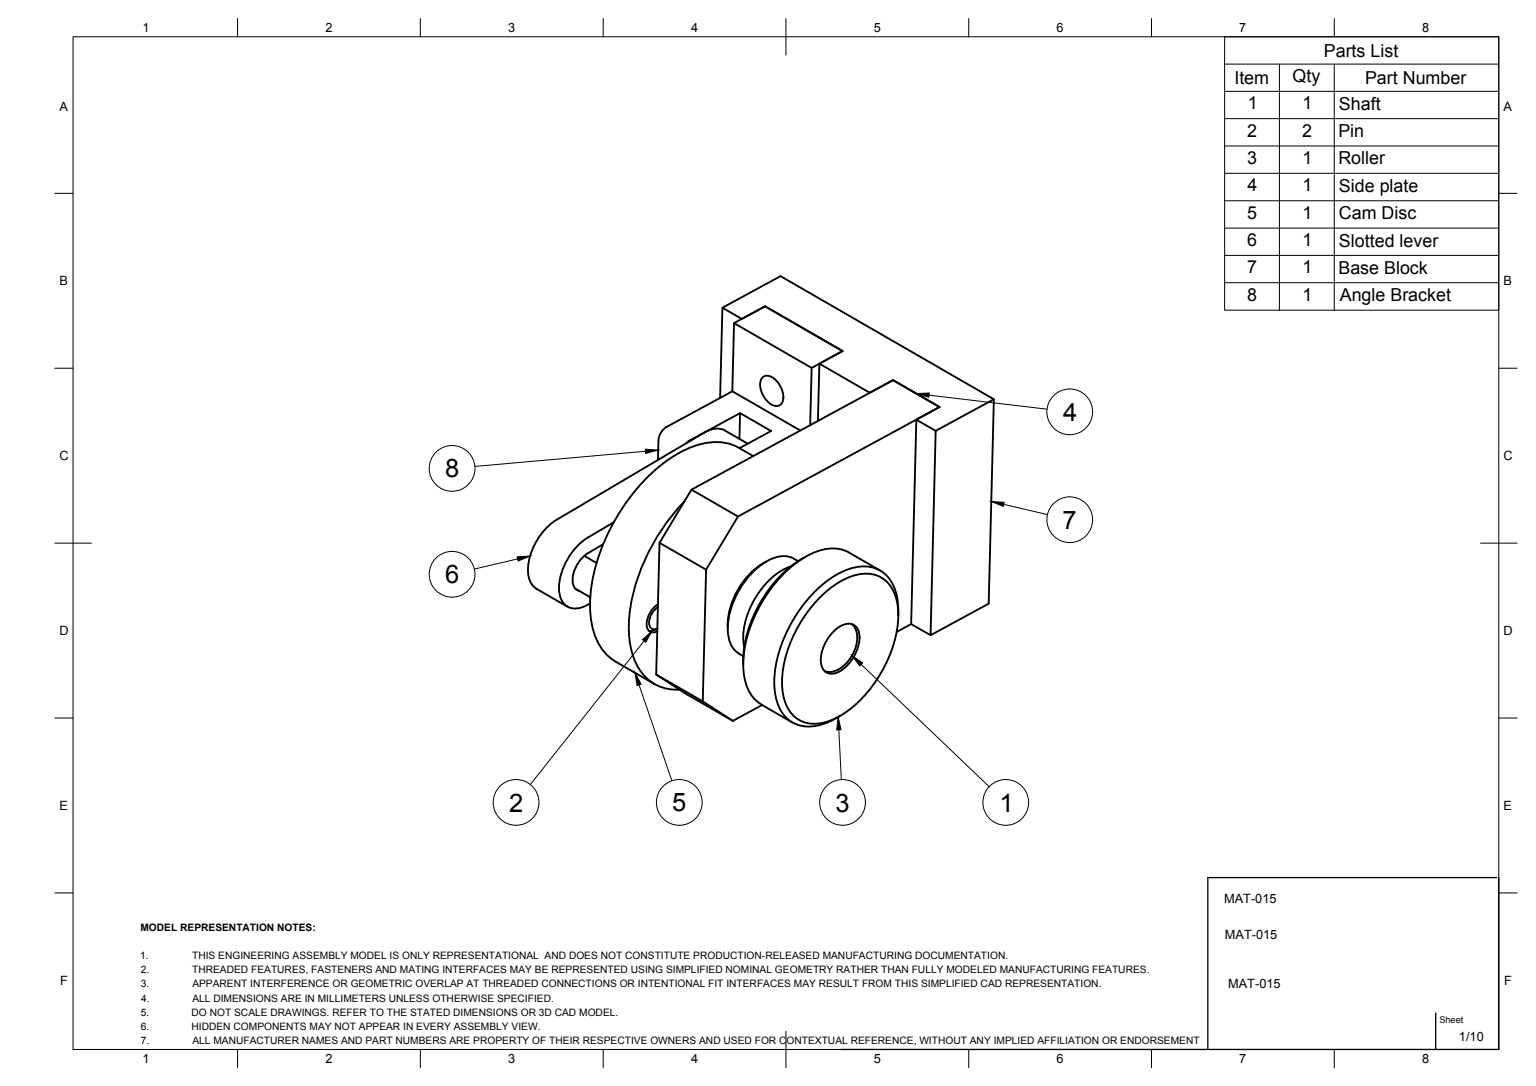
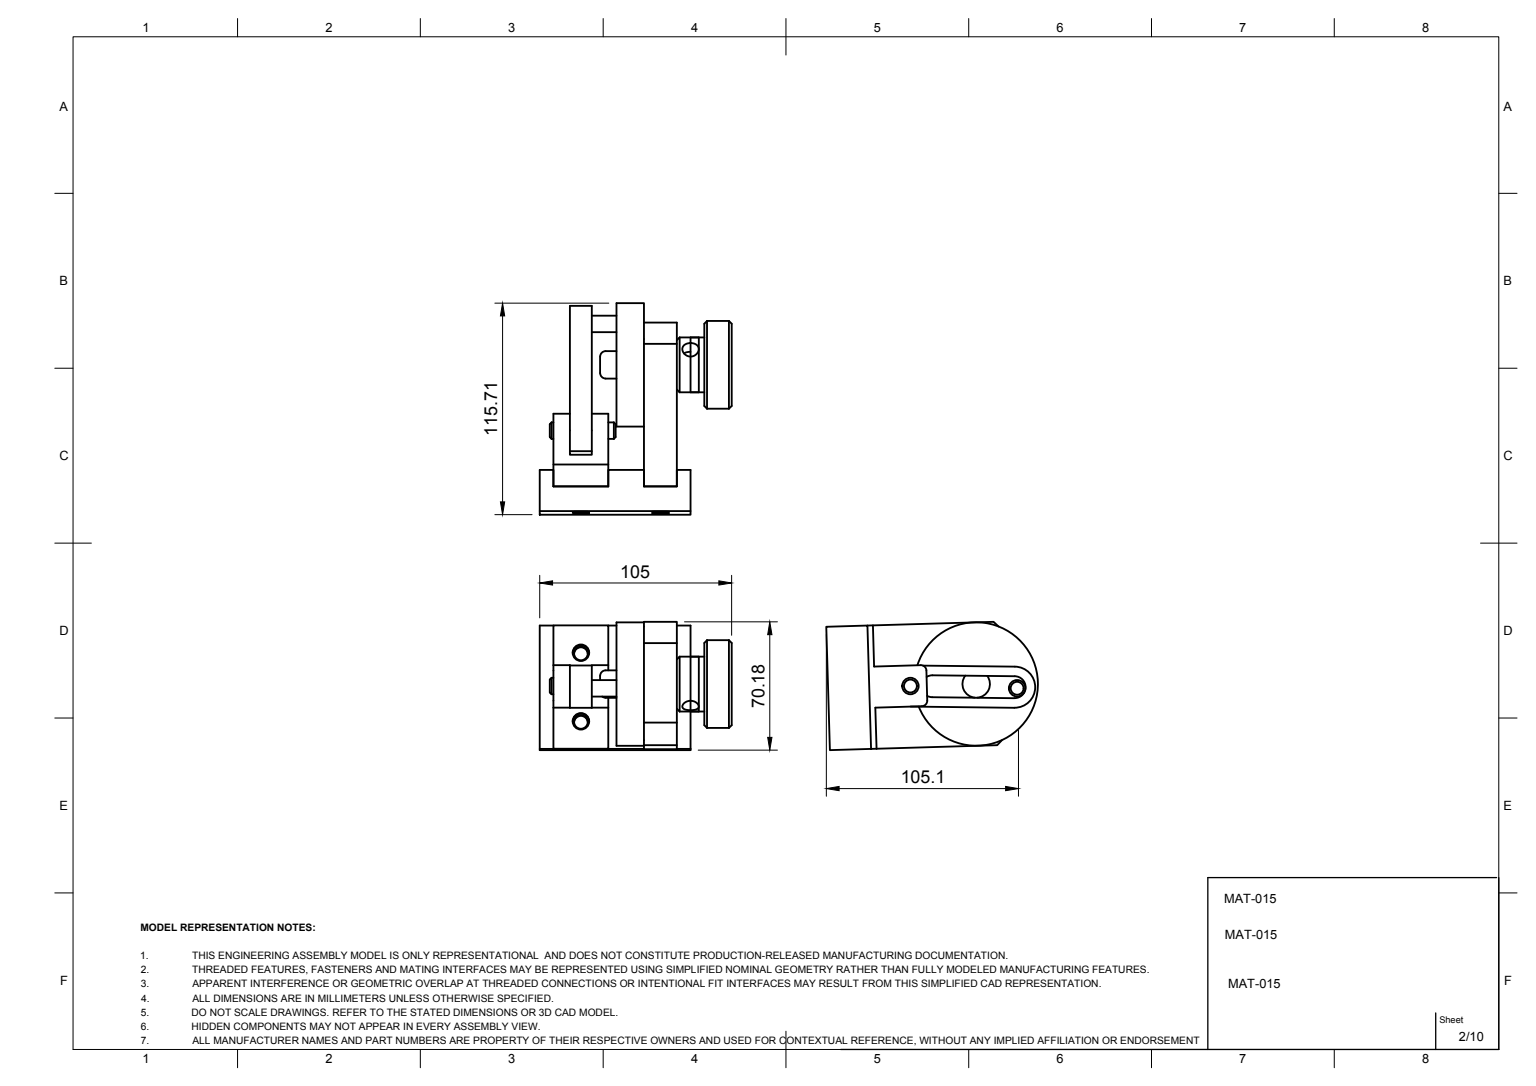
ISO-10303-21;
HEADER;
/* Generated by software containing ST-Developer
 * from STEP Tools, Inc. (www.steptools.com) 
 */

FILE_DESCRIPTION(
/* description */ ('STEP AP214'),
/* implementation_level */ '2;1');

FILE_NAME(
/* name */ 'MAT-015.step',
/* time_stamp */ '2026-11-14T06:03:18-08:00',
/* author */ (''),
/* organization */ (''),
/* preprocessor_version */ 'ST-DEVELOPER v20.2',
/* originating_system */ 'Autodesk Translation Framework v15.17.0.0',
/* authorisation */ '');

FILE_SCHEMA (('AUTOMOTIVE_DESIGN { 1 0 10303 214 3 1 1 }'));
ENDSEC;

DATA;
#10=MECHANICAL_DESIGN_GEOMETRIC_PRESENTATION_REPRESENTATION('',(#72,#73,
#74,#75,#76,#77,#78,#79),#3206);
#11=ITEM_DEFINED_TRANSFORMATION($,$,#1877,#2066);
#12=ITEM_DEFINED_TRANSFORMATION($,$,#2055,#2067);
#13=ITEM_DEFINED_TRANSFORMATION($,$,#1903,#2068);
#14=ITEM_DEFINED_TRANSFORMATION($,$,#1925,#2069);
#15=ITEM_DEFINED_TRANSFORMATION($,$,#1949,#2070);
#16=ITEM_DEFINED_TRANSFORMATION($,$,#1961,#2071);
#17=ITEM_DEFINED_TRANSFORMATION($,$,#1983,#2072);
#18=ITEM_DEFINED_TRANSFORMATION($,$,#2016,#2073);
#19=ITEM_DEFINED_TRANSFORMATION($,$,#2055,#2074);
#20=(
REPRESENTATION_RELATIONSHIP($,$,#3239,#3238)
REPRESENTATION_RELATIONSHIP_WITH_TRANSFORMATION(#11)
SHAPE_REPRESENTATION_RELATIONSHIP()
);
#21=(
REPRESENTATION_RELATIONSHIP($,$,#3246,#3238)
REPRESENTATION_RELATIONSHIP_WITH_TRANSFORMATION(#12)
SHAPE_REPRESENTATION_RELATIONSHIP()
);
#22=(
REPRESENTATION_RELATIONSHIP($,$,#3240,#3238)
REPRESENTATION_RELATIONSHIP_WITH_TRANSFORMATION(#13)
SHAPE_REPRESENTATION_RELATIONSHIP()
);
#23=(
REPRESENTATION_RELATIONSHIP($,$,#3241,#3238)
REPRESENTATION_RELATIONSHIP_WITH_TRANSFORMATION(#14)
SHAPE_REPRESENTATION_RELATIONSHIP()
);
#24=(
REPRESENTATION_RELATIONSHIP($,$,#3242,#3238)
REPRESENTATION_RELATIONSHIP_WITH_TRANSFORMATION(#15)
SHAPE_REPRESENTATION_RELATIONSHIP()
);
#25=(
REPRESENTATION_RELATIONSHIP($,$,#3243,#3238)
REPRESENTATION_RELATIONSHIP_WITH_TRANSFORMATION(#16)
SHAPE_REPRESENTATION_RELATIONSHIP()
);
#26=(
REPRESENTATION_RELATIONSHIP($,$,#3244,#3238)
REPRESENTATION_RELATIONSHIP_WITH_TRANSFORMATION(#17)
SHAPE_REPRESENTATION_RELATIONSHIP()
);
#27=(
REPRESENTATION_RELATIONSHIP($,$,#3245,#3238)
REPRESENTATION_RELATIONSHIP_WITH_TRANSFORMATION(#18)
SHAPE_REPRESENTATION_RELATIONSHIP()
);
#28=(
REPRESENTATION_RELATIONSHIP($,$,#3246,#3238)
REPRESENTATION_RELATIONSHIP_WITH_TRANSFORMATION(#19)
SHAPE_REPRESENTATION_RELATIONSHIP()
);
#29=CONTEXT_DEPENDENT_SHAPE_REPRESENTATION(#20,#3229);
#30=CONTEXT_DEPENDENT_SHAPE_REPRESENTATION(#21,#3230);
#31=CONTEXT_DEPENDENT_SHAPE_REPRESENTATION(#22,#3231);
#32=CONTEXT_DEPENDENT_SHAPE_REPRESENTATION(#23,#3232);
#33=CONTEXT_DEPENDENT_SHAPE_REPRESENTATION(#24,#3233);
#34=CONTEXT_DEPENDENT_SHAPE_REPRESENTATION(#25,#3234);
#35=CONTEXT_DEPENDENT_SHAPE_REPRESENTATION(#26,#3235);
#36=CONTEXT_DEPENDENT_SHAPE_REPRESENTATION(#27,#3236);
#37=CONTEXT_DEPENDENT_SHAPE_REPRESENTATION(#28,#3237);
#38=NEXT_ASSEMBLY_USAGE_OCCURRENCE('Shaft:1','Shaft:1','Shaft:1',#3248,
#3249,'Shaft:1');
#39=NEXT_ASSEMBLY_USAGE_OCCURRENCE('Pin:1','Pin:1','Pin:1',#3248,#3256,
'Pin:1');
#40=NEXT_ASSEMBLY_USAGE_OCCURRENCE('Roller:1','Roller:1','Roller:1',#3248,
#3250,'Roller:1');
#41=NEXT_ASSEMBLY_USAGE_OCCURRENCE('Side Plate:1','Side Plate:1',
'Side Plate:1',#3248,#3251,'Side Plate:1');
#42=NEXT_ASSEMBLY_USAGE_OCCURRENCE('Cam Disc:1','Cam Disc:1',
'Cam Disc:1',#3248,#3252,'Cam Disc:1');
#43=NEXT_ASSEMBLY_USAGE_OCCURRENCE('Slotted Lever:1','Slotted Lever:1',
'Slotted Lever:1',#3248,#3253,'Slotted Lever:1');
#44=NEXT_ASSEMBLY_USAGE_OCCURRENCE('Base Block:1','Base Block:1',
'Base Block:1',#3248,#3254,'Base Block:1');
#45=NEXT_ASSEMBLY_USAGE_OCCURRENCE('Angle Bracket:1','Angle Bracket:1',
'Angle Bracket:1',#3248,#3255,'Angle Bracket:1');
#46=NEXT_ASSEMBLY_USAGE_OCCURRENCE('Pin:2','Pin:2','Pin:2',#3248,#3256,
'Pin:2');
#47=B_SPLINE_CURVE_WITH_KNOTS('',3,(#2691,#2692,#2693,#2694,#2695,#2696,
#2697,#2698,#2699,#2700,#2701,#2702,#2703,#2704,#2705,#2706,#2707,#2708),
 .UNSPECIFIED.,.F.,.F.,(4,2,2,2,2,2,2,2,4),(-1.36519473470625,-1.19451997041109,
-1.02384520611593,-0.853221286734528,-0.682597367353127,-0.511973447971726,
-0.341349528590325,-0.170674764295162,0.),.UNSPECIFIED.);
#48=B_SPLINE_CURVE_WITH_KNOTS('',3,(#2712,#2713,#2714,#2715,#2716,#2717,
#2718,#2719,#2720,#2721,#2722,#2723,#2724,#2725,#2726,#2727,#2728,#2729),
 .UNSPECIFIED.,.F.,.F.,(4,2,2,2,2,2,2,2,4),(-1.39899108486948,-1.22355122072177,
-1.04811135657406,-0.873803449504402,-0.699495542434742,-0.525187635365083,
-0.350879728295424,-0.175439864147712,0.),.UNSPECIFIED.);
#49=B_SPLINE_CURVE_WITH_KNOTS('',3,(#2730,#2731,#2732,#2733,#2734,#2735,
#2736,#2737,#2738,#2739,#2740,#2741,#2742,#2743,#2744,#2745,#2746,#2747),
 .UNSPECIFIED.,.F.,.F.,(4,2,2,2,2,2,2,2,4),(-2.79798216973897,-2.62254230559126,
-2.44710244144355,-2.27279453437389,-2.09848662730423,-1.92417872023457,
-1.74987081316491,-1.5744309490172,-1.39899108486948),.UNSPECIFIED.);
#50=B_SPLINE_CURVE_WITH_KNOTS('',3,(#2748,#2749,#2750,#2751,#2752,#2753,
#2754,#2755,#2756,#2757,#2758,#2759,#2760,#2761,#2762,#2763,#2764,#2765),
 .UNSPECIFIED.,.F.,.F.,(4,2,2,2,2,2,2,2,4),(0.,0.170674764295163,0.341349528590325,
0.511973447971726,0.682597367353127,0.853221286734528,1.02384520611593,
1.19451997041109,1.36519473470625),.UNSPECIFIED.);
#51=CONICAL_SURFACE('',#1904,13.5,0.785398163397445);
#52=CONICAL_SURFACE('',#1908,22.5,0.785398163397448);
#53=CONICAL_SURFACE('',#1912,24.,0.785398163397452);
#54=CONICAL_SURFACE('',#2056,4.50000000000002,0.785398163397454);
#55=CONICAL_SURFACE('',#2059,3.54000000000001,0.785398163397446);
#56=SHAPE_REPRESENTATION_RELATIONSHIP('SRR','None',#3239,#64);
#57=SHAPE_REPRESENTATION_RELATIONSHIP('SRR','None',#3240,#65);
#58=SHAPE_REPRESENTATION_RELATIONSHIP('SRR','None',#3241,#66);
#59=SHAPE_REPRESENTATION_RELATIONSHIP('SRR','None',#3242,#67);
#60=SHAPE_REPRESENTATION_RELATIONSHIP('SRR','None',#3243,#68);
#61=SHAPE_REPRESENTATION_RELATIONSHIP('SRR','None',#3244,#69);
#62=SHAPE_REPRESENTATION_RELATIONSHIP('SRR','None',#3245,#70);
#63=SHAPE_REPRESENTATION_RELATIONSHIP('SRR','None',#3246,#71);
#64=ADVANCED_BREP_SHAPE_REPRESENTATION('',(#80),#3198);
#65=ADVANCED_BREP_SHAPE_REPRESENTATION('',(#81),#3199);
#66=ADVANCED_BREP_SHAPE_REPRESENTATION('',(#82),#3200);
#67=ADVANCED_BREP_SHAPE_REPRESENTATION('',(#83),#3201);
#68=ADVANCED_BREP_SHAPE_REPRESENTATION('',(#84),#3202);
#69=ADVANCED_BREP_SHAPE_REPRESENTATION('',(#85),#3203);
#70=ADVANCED_BREP_SHAPE_REPRESENTATION('',(#86),#3204);
#71=ADVANCED_BREP_SHAPE_REPRESENTATION('',(#87),#3205);
#72=STYLED_ITEM('',(#3288),#80);
#73=STYLED_ITEM('',(#3288),#81);
#74=STYLED_ITEM('',(#3288),#82);
#75=STYLED_ITEM('',(#3289),#83);
#76=STYLED_ITEM('',(#3288),#84);
#77=STYLED_ITEM('',(#3289),#85);
#78=STYLED_ITEM('',(#3290),#86);
#79=STYLED_ITEM('',(#3290),#87);
#80=MANIFOLD_SOLID_BREP('Body1',#1779);
#81=MANIFOLD_SOLID_BREP('Body1',#1780);
#82=MANIFOLD_SOLID_BREP('Body1',#1781);
#83=MANIFOLD_SOLID_BREP('Body1',#1782);
#84=MANIFOLD_SOLID_BREP('Body1',#1783);
#85=MANIFOLD_SOLID_BREP('Body1',#1784);
#86=MANIFOLD_SOLID_BREP('Body1',#1785);
#87=MANIFOLD_SOLID_BREP('Body1',#1786);
#88=PLANE('',#1896);
#89=PLANE('',#1897);
#90=PLANE('',#1898);
#91=PLANE('',#1899);
#92=PLANE('',#1900);
#93=PLANE('',#1901);
#94=PLANE('',#1902);
#95=PLANE('',#1922);
#96=PLANE('',#1923);
#97=PLANE('',#1924);
#98=PLANE('',#1938);
#99=PLANE('',#1939);
#100=PLANE('',#1940);
#101=PLANE('',#1941);
#102=PLANE('',#1942);
#103=PLANE('',#1943);
#104=PLANE('',#1944);
#105=PLANE('',#1945);
#106=PLANE('',#1946);
#107=PLANE('',#1947);
#108=PLANE('',#1948);
#109=PLANE('',#1959);
#110=PLANE('',#1960);
#111=PLANE('',#1971);
#112=PLANE('',#1974);
#113=PLANE('',#1978);
#114=PLANE('',#1979);
#115=PLANE('',#1981);
#116=PLANE('',#1982);
#117=PLANE('',#2002);
#118=PLANE('',#2003);
#119=PLANE('',#2004);
#120=PLANE('',#2005);
#121=PLANE('',#2006);
#122=PLANE('',#2007);
#123=PLANE('',#2008);
#124=PLANE('',#2009);
#125=PLANE('',#2010);
#126=PLANE('',#2011);
#127=PLANE('',#2012);
#128=PLANE('',#2013);
#129=PLANE('',#2014);
#130=PLANE('',#2015);
#131=PLANE('',#2029);
#132=PLANE('',#2030);
#133=PLANE('',#2031);
#134=PLANE('',#2032);
#135=PLANE('',#2033);
#136=PLANE('',#2034);
#137=PLANE('',#2037);
#138=PLANE('',#2038);
#139=PLANE('',#2041);
#140=PLANE('',#2042);
#141=PLANE('',#2043);
#142=PLANE('',#2044);
#143=PLANE('',#2047);
#144=PLANE('',#2050);
#145=PLANE('',#2064);
#146=PLANE('',#2065);
#147=FACE_BOUND('',#617,.T.);
#148=FACE_BOUND('',#620,.T.);
#149=FACE_BOUND('',#622,.T.);
#150=FACE_BOUND('',#633,.T.);
#151=FACE_BOUND('',#635,.T.);
#152=FACE_BOUND('',#637,.T.);
#153=FACE_BOUND('',#639,.T.);
#154=FACE_BOUND('',#641,.T.);
#155=FACE_BOUND('',#647,.T.);
#156=FACE_BOUND('',#649,.T.);
#157=FACE_BOUND('',#652,.T.);
#158=FACE_BOUND('',#653,.T.);
#159=FACE_BOUND('',#654,.T.);
#160=FACE_BOUND('',#666,.T.);
#161=FACE_BOUND('',#667,.T.);
#162=FACE_BOUND('',#669,.T.);
#163=FACE_BOUND('',#670,.T.);
#164=FACE_BOUND('',#675,.T.);
#165=FACE_BOUND('',#676,.T.);
#166=FACE_BOUND('',#678,.T.);
#167=FACE_BOUND('',#679,.T.);
#168=FACE_BOUND('',#693,.T.);
#169=FACE_BOUND('',#694,.T.);
#170=FACE_BOUND('',#695,.T.);
#171=FACE_BOUND('',#697,.T.);
#172=FACE_BOUND('',#698,.T.);
#173=FACE_BOUND('',#699,.T.);
#174=FACE_BOUND('',#701,.T.);
#175=FACE_BOUND('',#702,.T.);
#176=FACE_BOUND('',#703,.T.);
#177=FACE_BOUND('',#704,.T.);
#178=FACE_BOUND('',#705,.T.);
#179=FACE_BOUND('',#706,.T.);
#180=FACE_BOUND('',#724,.T.);
#181=FACE_BOUND('',#726,.T.);
#182=FACE_BOUND('',#728,.T.);
#183=FACE_BOUND('',#729,.T.);
#184=FACE_BOUND('',#732,.T.);
#185=FACE_BOUND('',#735,.T.);
#186=FACE_BOUND('',#740,.T.);
#187=FACE_BOUND('',#742,.T.);
#188=LINE('',#2638,#333);
#189=LINE('',#2643,#334);
#190=LINE('',#2646,#335);
#191=LINE('',#2652,#336);
#192=LINE('',#2655,#337);
#193=LINE('',#2661,#338);
#194=LINE('',#2662,#339);
#195=LINE('',#2672,#340);
#196=LINE('',#2680,#341);
#197=LINE('',#2686,#342);
#198=LINE('',#2710,#343);
#199=LINE('',#2767,#344);
#200=LINE('',#2772,#345);
#201=LINE('',#2776,#346);
#202=LINE('',#2786,#347);
#203=LINE('',#2792,#348);
#204=LINE('',#2798,#349);
#205=LINE('',#2804,#350);
#206=LINE('',#2809,#351);
#207=LINE('',#2811,#352);
#208=LINE('',#2813,#353);
#209=LINE('',#2815,#354);
#210=LINE('',#2817,#355);
#211=LINE('',#2818,#356);
#212=LINE('',#2822,#357);
#213=LINE('',#2824,#358);
#214=LINE('',#2826,#359);
#215=LINE('',#2828,#360);
#216=LINE('',#2830,#361);
#217=LINE('',#2831,#362);
#218=LINE('',#2833,#363);
#219=LINE('',#2834,#364);
#220=LINE('',#2836,#365);
#221=LINE('',#2838,#366);
#222=LINE('',#2840,#367);
#223=LINE('',#2841,#368);
#224=LINE('',#2852,#369);
#225=LINE('',#2858,#370);
#226=LINE('',#2864,#371);
#227=LINE('',#2874,#372);
#228=LINE('',#2877,#373);
#229=LINE('',#2882,#374);
#230=LINE('',#2889,#375);
#231=LINE('',#2892,#376);
#232=LINE('',#2897,#377);
#233=LINE('',#2898,#378);
#234=LINE('',#2902,#379);
#235=LINE('',#2903,#380);
#236=LINE('',#2908,#381);
#237=LINE('',#2909,#382);
#238=LINE('',#2911,#383);
#239=LINE('',#2914,#384);
#240=LINE('',#2916,#385);
#241=LINE('',#2917,#386);
#242=LINE('',#2921,#387);
#243=LINE('',#2922,#388);
#244=LINE('',#2930,#389);
#245=LINE('',#2936,#390);
#246=LINE('',#2942,#391);
#247=LINE('',#2948,#392);
#248=LINE('',#2954,#393);
#249=LINE('',#2960,#394);
#250=LINE('',#2965,#395);
#251=LINE('',#2967,#396);
#252=LINE('',#2969,#397);
#253=LINE('',#2970,#398);
#254=LINE('',#2974,#399);
#255=LINE('',#2976,#400);
#256=LINE('',#2978,#401);
#257=LINE('',#2979,#402);
#258=LINE('',#2983,#403);
#259=LINE('',#2985,#404);
#260=LINE('',#2987,#405);
#261=LINE('',#2988,#406);
#262=LINE('',#2991,#407);
#263=LINE('',#2993,#408);
#264=LINE('',#2994,#409);
#265=LINE('',#2997,#410);
#266=LINE('',#2999,#411);
#267=LINE('',#3000,#412);
#268=LINE('',#3002,#413);
#269=LINE('',#3004,#414);
#270=LINE('',#3005,#415);
#271=LINE('',#3007,#416);
#272=LINE('',#3008,#417);
#273=LINE('',#3011,#418);
#274=LINE('',#3012,#419);
#275=LINE('',#3015,#420);
#276=LINE('',#3016,#421);
#277=LINE('',#3018,#422);
#278=LINE('',#3020,#423);
#279=LINE('',#3021,#424);
#280=LINE('',#3023,#425);
#281=LINE('',#3024,#426);
#282=LINE('',#3026,#427);
#283=LINE('',#3028,#428);
#284=LINE('',#3031,#429);
#285=LINE('',#3034,#430);
#286=LINE('',#3041,#431);
#287=LINE('',#3047,#432);
#288=LINE('',#3053,#433);
#289=LINE('',#3059,#434);
#290=LINE('',#3064,#435);
#291=LINE('',#3066,#436);
#292=LINE('',#3068,#437);
#293=LINE('',#3069,#438);
#294=LINE('',#3073,#439);
#295=LINE('',#3075,#440);
#296=LINE('',#3077,#441);
#297=LINE('',#3078,#442);
#298=LINE('',#3082,#443);
#299=LINE('',#3084,#444);
#300=LINE('',#3086,#445);
#301=LINE('',#3087,#446);
#302=LINE('',#3091,#447);
#303=LINE('',#3093,#448);
#304=LINE('',#3095,#449);
#305=LINE('',#3096,#450);
#306=LINE('',#3098,#451);
#307=LINE('',#3099,#452);
#308=LINE('',#3102,#453);
#309=LINE('',#3106,#454);
#310=LINE('',#3107,#455);
#311=LINE('',#3109,#456);
#312=LINE('',#3113,#457);
#313=LINE('',#3116,#458);
#314=LINE('',#3118,#459);
#315=LINE('',#3123,#460);
#316=LINE('',#3124,#461);
#317=LINE('',#3126,#462);
#318=LINE('',#3128,#463);
#319=LINE('',#3129,#464);
#320=LINE('',#3132,#465);
#321=LINE('',#3134,#466);
#322=LINE('',#3136,#467);
#323=LINE('',#3138,#468);
#324=LINE('',#3139,#469);
#325=LINE('',#3143,#470);
#326=LINE('',#3144,#471);
#327=LINE('',#3145,#472);
#328=LINE('',#3148,#473);
#329=LINE('',#3153,#474);
#330=LINE('',#3164,#475);
#331=LINE('',#3172,#476);
#332=LINE('',#3175,#477);
#333=VECTOR('',#2101,15.);
#334=VECTOR('',#2108,7.5);
#335=VECTOR('',#2111,7.49999999999999);
#336=VECTOR('',#2116,1000.);
#337=VECTOR('',#2119,1000.);
#338=VECTOR('',#2130,1000.);
#339=VECTOR('',#2131,1000.);
#340=VECTOR('',#2144,13.5);
#341=VECTOR('',#2153,22.5);
#342=VECTOR('',#2160,24.);
#343=VECTOR('',#2165,4.5);
#344=VECTOR('',#2168,24.);
#345=VECTOR('',#2173,7.5);
#346=VECTOR('',#2178,15.);
#347=VECTOR('',#2193,4.5);
#348=VECTOR('',#2200,3.75);
#349=VECTOR('',#2207,3.75);
#350=VECTOR('',#2214,7.50000000000001);
#351=VECTOR('',#2219,1000.);
#352=VECTOR('',#2220,1000.);
#353=VECTOR('',#2221,1000.);
#354=VECTOR('',#2222,1000.);
#355=VECTOR('',#2223,1000.);
#356=VECTOR('',#2224,1000.);
#357=VECTOR('',#2227,1000.);
#358=VECTOR('',#2228,1000.);
#359=VECTOR('',#2229,1000.);
#360=VECTOR('',#2230,1000.);
#361=VECTOR('',#2231,1000.);
#362=VECTOR('',#2232,1000.);
#363=VECTOR('',#2235,1000.);
#364=VECTOR('',#2236,1000.);
#365=VECTOR('',#2239,1000.);
#366=VECTOR('',#2242,1000.);
#367=VECTOR('',#2245,1000.);
#368=VECTOR('',#2246,1000.);
#369=VECTOR('',#2263,4.50000000000001);
#370=VECTOR('',#2270,7.50000000000002);
#371=VECTOR('',#2277,33.7500000000001);
#372=VECTOR('',#2290,1000.);
#373=VECTOR('',#2293,1000.);
#374=VECTOR('',#2298,4.5);
#375=VECTOR('',#2305,1000.);
#376=VECTOR('',#2308,1000.);
#377=VECTOR('',#2313,1000.);
#378=VECTOR('',#2314,1000.);
#379=VECTOR('',#2317,1000.);
#380=VECTOR('',#2318,1000.);
#381=VECTOR('',#2323,1000.);
#382=VECTOR('',#2324,1000.);
#383=VECTOR('',#2325,1000.);
#384=VECTOR('',#2328,1000.);
#385=VECTOR('',#2331,1000.);
#386=VECTOR('',#2332,1000.);
#387=VECTOR('',#2339,1000.);
#388=VECTOR('',#2340,1000.);
#389=VECTOR('',#2351,4.5);
#390=VECTOR('',#2358,4.5);
#391=VECTOR('',#2365,4.5);
#392=VECTOR('',#2372,4.5);
#393=VECTOR('',#2379,3.75);
#394=VECTOR('',#2386,3.75);
#395=VECTOR('',#2391,1000.);
#396=VECTOR('',#2392,1000.);
#397=VECTOR('',#2393,1000.);
#398=VECTOR('',#2394,1000.);
#399=VECTOR('',#2397,1000.);
#400=VECTOR('',#2398,1000.);
#401=VECTOR('',#2399,1000.);
#402=VECTOR('',#2400,1000.);
#403=VECTOR('',#2403,1000.);
#404=VECTOR('',#2404,1000.);
#405=VECTOR('',#2405,1000.);
#406=VECTOR('',#2406,1000.);
#407=VECTOR('',#2409,1000.);
#408=VECTOR('',#2410,1000.);
#409=VECTOR('',#2411,1000.);
#410=VECTOR('',#2414,1000.);
#411=VECTOR('',#2415,1000.);
#412=VECTOR('',#2416,1000.);
#413=VECTOR('',#2417,1000.);
#414=VECTOR('',#2418,1000.);
#415=VECTOR('',#2419,1000.);
#416=VECTOR('',#2420,1000.);
#417=VECTOR('',#2421,1000.);
#418=VECTOR('',#2424,1000.);
#419=VECTOR('',#2425,1000.);
#420=VECTOR('',#2428,1000.);
#421=VECTOR('',#2429,1000.);
#422=VECTOR('',#2430,1000.);
#423=VECTOR('',#2431,1000.);
#424=VECTOR('',#2432,1000.);
#425=VECTOR('',#2433,1000.);
#426=VECTOR('',#2434,1000.);
#427=VECTOR('',#2437,1000.);
#428=VECTOR('',#2440,1000.);
#429=VECTOR('',#2445,1000.);
#430=VECTOR('',#2450,1000.);
#431=VECTOR('',#2459,4.50000000000001);
#432=VECTOR('',#2466,4.50000000000001);
#433=VECTOR('',#2473,4.50000000000002);
#434=VECTOR('',#2480,4.50000000000001);
#435=VECTOR('',#2485,1000.);
#436=VECTOR('',#2486,1000.);
#437=VECTOR('',#2487,1000.);
#438=VECTOR('',#2488,1000.);
#439=VECTOR('',#2491,1000.);
#440=VECTOR('',#2492,1000.);
#441=VECTOR('',#2493,1000.);
#442=VECTOR('',#2494,1000.);
#443=VECTOR('',#2497,1000.);
#444=VECTOR('',#2498,1000.);
#445=VECTOR('',#2499,1000.);
#446=VECTOR('',#2500,1000.);
#447=VECTOR('',#2503,1000.);
#448=VECTOR('',#2504,1000.);
#449=VECTOR('',#2505,1000.);
#450=VECTOR('',#2506,1000.);
#451=VECTOR('',#2509,1000.);
#452=VECTOR('',#2510,1000.);
#453=VECTOR('',#2513,1000.);
#454=VECTOR('',#2518,1000.);
#455=VECTOR('',#2519,1000.);
#456=VECTOR('',#2522,1000.);
#457=VECTOR('',#2525,1000.);
#458=VECTOR('',#2528,1000.);
#459=VECTOR('',#2529,1000.);
#460=VECTOR('',#2534,1000.);
#461=VECTOR('',#2535,1000.);
#462=VECTOR('',#2536,1000.);
#463=VECTOR('',#2537,1000.);
#464=VECTOR('',#2538,1000.);
#465=VECTOR('',#2541,1000.);
#466=VECTOR('',#2542,1000.);
#467=VECTOR('',#2543,1000.);
#468=VECTOR('',#2544,1000.);
#469=VECTOR('',#2545,1000.);
#470=VECTOR('',#2548,1000.);
#471=VECTOR('',#2549,1000.);
#472=VECTOR('',#2550,1000.);
#473=VECTOR('',#2555,1000.);
#474=VECTOR('',#2564,1000.);
#475=VECTOR('',#2581,4.50000000000002);
#476=VECTOR('',#2590,3.54000000000001);
#477=VECTOR('',#2595,4.50000000000002);
#478=CYLINDRICAL_SURFACE('',#1887,15.);
#479=CYLINDRICAL_SURFACE('',#1890,7.5);
#480=CYLINDRICAL_SURFACE('',#1892,7.49999999999999);
#481=CYLINDRICAL_SURFACE('',#1915,4.5);
#482=CYLINDRICAL_SURFACE('',#1916,24.);
#483=CYLINDRICAL_SURFACE('',#1917,7.5);
#484=CYLINDRICAL_SURFACE('',#1920,15.);
#485=CYLINDRICAL_SURFACE('',#1926,4.5);
#486=CYLINDRICAL_SURFACE('',#1929,3.75);
#487=CYLINDRICAL_SURFACE('',#1932,3.75);
#488=CYLINDRICAL_SURFACE('',#1935,7.50000000000001);
#489=CYLINDRICAL_SURFACE('',#1950,4.50000000000001);
#490=CYLINDRICAL_SURFACE('',#1953,7.50000000000002);
#491=CYLINDRICAL_SURFACE('',#1956,33.7500000000001);
#492=CYLINDRICAL_SURFACE('',#1962,6.);
#493=CYLINDRICAL_SURFACE('',#1965,4.5);
#494=CYLINDRICAL_SURFACE('',#1968,11.25);
#495=CYLINDRICAL_SURFACE('',#1977,11.25);
#496=CYLINDRICAL_SURFACE('',#1980,6.);
#497=CYLINDRICAL_SURFACE('',#1984,4.5);
#498=CYLINDRICAL_SURFACE('',#1987,4.5);
#499=CYLINDRICAL_SURFACE('',#1990,4.5);
#500=CYLINDRICAL_SURFACE('',#1993,4.5);
#501=CYLINDRICAL_SURFACE('',#1996,3.75);
#502=CYLINDRICAL_SURFACE('',#1999,3.75);
#503=CYLINDRICAL_SURFACE('',#2017,4.50000000000001);
#504=CYLINDRICAL_SURFACE('',#2020,4.50000000000001);
#505=CYLINDRICAL_SURFACE('',#2023,4.50000000000002);
#506=CYLINDRICAL_SURFACE('',#2026,4.50000000000001);
#507=CYLINDRICAL_SURFACE('',#2051,3.00000000000001);
#508=CYLINDRICAL_SURFACE('',#2052,3.00000000000001);
#509=CYLINDRICAL_SURFACE('',#2053,3.00000000000001);
#510=CYLINDRICAL_SURFACE('',#2054,3.00000000000001);
#511=CYLINDRICAL_SURFACE('',#2063,4.50000000000002);
#512=FACE_OUTER_BOUND('',#612,.T.);
#513=FACE_OUTER_BOUND('',#613,.T.);
#514=FACE_OUTER_BOUND('',#614,.T.);
#515=FACE_OUTER_BOUND('',#615,.T.);
#516=FACE_OUTER_BOUND('',#616,.T.);
#517=FACE_OUTER_BOUND('',#618,.T.);
#518=FACE_OUTER_BOUND('',#619,.T.);
#519=FACE_OUTER_BOUND('',#621,.T.);
#520=FACE_OUTER_BOUND('',#623,.T.);
#521=FACE_OUTER_BOUND('',#624,.T.);
#522=FACE_OUTER_BOUND('',#625,.T.);
#523=FACE_OUTER_BOUND('',#626,.T.);
#524=FACE_OUTER_BOUND('',#627,.T.);
#525=FACE_OUTER_BOUND('',#628,.T.);
#526=FACE_OUTER_BOUND('',#629,.T.);
#527=FACE_OUTER_BOUND('',#630,.T.);
#528=FACE_OUTER_BOUND('',#631,.T.);
#529=FACE_OUTER_BOUND('',#632,.T.);
#530=FACE_OUTER_BOUND('',#634,.T.);
#531=FACE_OUTER_BOUND('',#636,.T.);
#532=FACE_OUTER_BOUND('',#638,.T.);
#533=FACE_OUTER_BOUND('',#640,.T.);
#534=FACE_OUTER_BOUND('',#642,.T.);
#535=FACE_OUTER_BOUND('',#643,.T.);
#536=FACE_OUTER_BOUND('',#644,.T.);
#537=FACE_OUTER_BOUND('',#645,.T.);
#538=FACE_OUTER_BOUND('',#646,.T.);
#539=FACE_OUTER_BOUND('',#648,.T.);
#540=FACE_OUTER_BOUND('',#650,.T.);
#541=FACE_OUTER_BOUND('',#651,.T.);
#542=FACE_OUTER_BOUND('',#655,.T.);
#543=FACE_OUTER_BOUND('',#656,.T.);
#544=FACE_OUTER_BOUND('',#657,.T.);
#545=FACE_OUTER_BOUND('',#658,.T.);
#546=FACE_OUTER_BOUND('',#659,.T.);
#547=FACE_OUTER_BOUND('',#660,.T.);
#548=FACE_OUTER_BOUND('',#661,.T.);
#549=FACE_OUTER_BOUND('',#662,.T.);
#550=FACE_OUTER_BOUND('',#663,.T.);
#551=FACE_OUTER_BOUND('',#664,.T.);
#552=FACE_OUTER_BOUND('',#665,.T.);
#553=FACE_OUTER_BOUND('',#668,.T.);
#554=FACE_OUTER_BOUND('',#671,.T.);
#555=FACE_OUTER_BOUND('',#672,.T.);
#556=FACE_OUTER_BOUND('',#673,.T.);
#557=FACE_OUTER_BOUND('',#674,.T.);
#558=FACE_OUTER_BOUND('',#677,.T.);
#559=FACE_OUTER_BOUND('',#680,.T.);
#560=FACE_OUTER_BOUND('',#681,.T.);
#561=FACE_OUTER_BOUND('',#682,.T.);
#562=FACE_OUTER_BOUND('',#683,.T.);
#563=FACE_OUTER_BOUND('',#684,.T.);
#564=FACE_OUTER_BOUND('',#685,.T.);
#565=FACE_OUTER_BOUND('',#686,.T.);
#566=FACE_OUTER_BOUND('',#687,.T.);
#567=FACE_OUTER_BOUND('',#688,.T.);
#568=FACE_OUTER_BOUND('',#689,.T.);
#569=FACE_OUTER_BOUND('',#690,.T.);
#570=FACE_OUTER_BOUND('',#691,.T.);
#571=FACE_OUTER_BOUND('',#692,.T.);
#572=FACE_OUTER_BOUND('',#696,.T.);
#573=FACE_OUTER_BOUND('',#700,.T.);
#574=FACE_OUTER_BOUND('',#707,.T.);
#575=FACE_OUTER_BOUND('',#708,.T.);
#576=FACE_OUTER_BOUND('',#709,.T.);
#577=FACE_OUTER_BOUND('',#710,.T.);
#578=FACE_OUTER_BOUND('',#711,.T.);
#579=FACE_OUTER_BOUND('',#712,.T.);
#580=FACE_OUTER_BOUND('',#713,.T.);
#581=FACE_OUTER_BOUND('',#714,.T.);
#582=FACE_OUTER_BOUND('',#715,.T.);
#583=FACE_OUTER_BOUND('',#716,.T.);
#584=FACE_OUTER_BOUND('',#717,.T.);
#585=FACE_OUTER_BOUND('',#718,.T.);
#586=FACE_OUTER_BOUND('',#719,.T.);
#587=FACE_OUTER_BOUND('',#720,.T.);
#588=FACE_OUTER_BOUND('',#721,.T.);
#589=FACE_OUTER_BOUND('',#722,.T.);
#590=FACE_OUTER_BOUND('',#723,.T.);
#591=FACE_OUTER_BOUND('',#725,.T.);
#592=FACE_OUTER_BOUND('',#727,.T.);
#593=FACE_OUTER_BOUND('',#730,.T.);
#594=FACE_OUTER_BOUND('',#731,.T.);
#595=FACE_OUTER_BOUND('',#733,.T.);
#596=FACE_OUTER_BOUND('',#734,.T.);
#597=FACE_OUTER_BOUND('',#736,.T.);
#598=FACE_OUTER_BOUND('',#737,.T.);
#599=FACE_OUTER_BOUND('',#738,.T.);
#600=FACE_OUTER_BOUND('',#739,.T.);
#601=FACE_OUTER_BOUND('',#741,.T.);
#602=FACE_OUTER_BOUND('',#743,.T.);
#603=FACE_OUTER_BOUND('',#744,.T.);
#604=FACE_OUTER_BOUND('',#745,.T.);
#605=FACE_OUTER_BOUND('',#746,.T.);
#606=FACE_OUTER_BOUND('',#747,.T.);
#607=FACE_OUTER_BOUND('',#748,.T.);
#608=FACE_OUTER_BOUND('',#749,.T.);
#609=FACE_OUTER_BOUND('',#750,.T.);
#610=FACE_OUTER_BOUND('',#751,.T.);
#611=FACE_OUTER_BOUND('',#752,.T.);
#612=EDGE_LOOP('',(#1217,#1218,#1219,#1220));
#613=EDGE_LOOP('',(#1221,#1222,#1223,#1224,#1225));
#614=EDGE_LOOP('',(#1226,#1227,#1228,#1229));
#615=EDGE_LOOP('',(#1230,#1231,#1232,#1233));
#616=EDGE_LOOP('',(#1234,#1235,#1236,#1237,#1238));
#617=EDGE_LOOP('',(#1239,#1240,#1241,#1242));
#618=EDGE_LOOP('',(#1243));
#619=EDGE_LOOP('',(#1244));
#620=EDGE_LOOP('',(#1245));
#621=EDGE_LOOP('',(#1246));
#622=EDGE_LOOP('',(#1247));
#623=EDGE_LOOP('',(#1248));
#624=EDGE_LOOP('',(#1249,#1250,#1251,#1252));
#625=EDGE_LOOP('',(#1253,#1254));
#626=EDGE_LOOP('',(#1255,#1256));
#627=EDGE_LOOP('',(#1257,#1258,#1259,#1260,#1261));
#628=EDGE_LOOP('',(#1262,#1263,#1264,#1265,#1266));
#629=EDGE_LOOP('',(#1267,#1268,#1269,#1270));
#630=EDGE_LOOP('',(#1271,#1272,#1273,#1274,#1275,#1276));
#631=EDGE_LOOP('',(#1277,#1278,#1279,#1280,#1281));
#632=EDGE_LOOP('',(#1282,#1283,#1284,#1285));
#633=EDGE_LOOP('',(#1286,#1287));
#634=EDGE_LOOP('',(#1288,#1289,#1290,#1291,#1292));
#635=EDGE_LOOP('',(#1293,#1294));
#636=EDGE_LOOP('',(#1295));
#637=EDGE_LOOP('',(#1296));
#638=EDGE_LOOP('',(#1297));
#639=EDGE_LOOP('',(#1298));
#640=EDGE_LOOP('',(#1299));
#641=EDGE_LOOP('',(#1300));
#642=EDGE_LOOP('',(#1301,#1302,#1303,#1304));
#643=EDGE_LOOP('',(#1305,#1306,#1307,#1308));
#644=EDGE_LOOP('',(#1309,#1310,#1311,#1312));
#645=EDGE_LOOP('',(#1313,#1314,#1315,#1316));
#646=EDGE_LOOP('',(#1317,#1318,#1319,#1320,#1321,#1322));
#647=EDGE_LOOP('',(#1323));
#648=EDGE_LOOP('',(#1324,#1325,#1326,#1327,#1328,#1329));
#649=EDGE_LOOP('',(#1330));
#650=EDGE_LOOP('',(#1331,#1332,#1333,#1334));
#651=EDGE_LOOP('',(#1335,#1336,#1337,#1338));
#652=EDGE_LOOP('',(#1339));
#653=EDGE_LOOP('',(#1340));
#654=EDGE_LOOP('',(#1341));
#655=EDGE_LOOP('',(#1342,#1343,#1344,#1345));
#656=EDGE_LOOP('',(#1346,#1347,#1348,#1349));
#657=EDGE_LOOP('',(#1350,#1351,#1352,#1353));
#658=EDGE_LOOP('',(#1354,#1355,#1356,#1357));
#659=EDGE_LOOP('',(#1358));
#660=EDGE_LOOP('',(#1359));
#661=EDGE_LOOP('',(#1360));
#662=EDGE_LOOP('',(#1361,#1362,#1363,#1364));
#663=EDGE_LOOP('',(#1365,#1366,#1367,#1368));
#664=EDGE_LOOP('',(#1369,#1370,#1371,#1372));
#665=EDGE_LOOP('',(#1373));
#666=EDGE_LOOP('',(#1374));
#667=EDGE_LOOP('',(#1375));
#668=EDGE_LOOP('',(#1376));
#669=EDGE_LOOP('',(#1377));
#670=EDGE_LOOP('',(#1378));
#671=EDGE_LOOP('',(#1379,#1380,#1381,#1382));
#672=EDGE_LOOP('',(#1383,#1384,#1385,#1386));
#673=EDGE_LOOP('',(#1387,#1388,#1389,#1390));
#674=EDGE_LOOP('',(#1391,#1392,#1393,#1394));
#675=EDGE_LOOP('',(#1395,#1396,#1397,#1398));
#676=EDGE_LOOP('',(#1399));
#677=EDGE_LOOP('',(#1400,#1401,#1402,#1403));
#678=EDGE_LOOP('',(#1404,#1405,#1406,#1407));
#679=EDGE_LOOP('',(#1408));
#680=EDGE_LOOP('',(#1409,#1410,#1411,#1412));
#681=EDGE_LOOP('',(#1413,#1414,#1415,#1416));
#682=EDGE_LOOP('',(#1417,#1418,#1419,#1420));
#683=EDGE_LOOP('',(#1421,#1422,#1423,#1424));
#684=EDGE_LOOP('',(#1425,#1426,#1427,#1428));
#685=EDGE_LOOP('',(#1429,#1430,#1431,#1432));
#686=EDGE_LOOP('',(#1433,#1434,#1435,#1436));
#687=EDGE_LOOP('',(#1437,#1438,#1439,#1440));
#688=EDGE_LOOP('',(#1441,#1442,#1443,#1444));
#689=EDGE_LOOP('',(#1445,#1446,#1447,#1448));
#690=EDGE_LOOP('',(#1449,#1450,#1451,#1452));
#691=EDGE_LOOP('',(#1453,#1454,#1455,#1456));
#692=EDGE_LOOP('',(#1457,#1458,#1459,#1460));
#693=EDGE_LOOP('',(#1461));
#694=EDGE_LOOP('',(#1462));
#695=EDGE_LOOP('',(#1463));
#696=EDGE_LOOP('',(#1464,#1465,#1466,#1467));
#697=EDGE_LOOP('',(#1468));
#698=EDGE_LOOP('',(#1469));
#699=EDGE_LOOP('',(#1470));
#700=EDGE_LOOP('',(#1471,#1472,#1473,#1474));
#701=EDGE_LOOP('',(#1475));
#702=EDGE_LOOP('',(#1476));
#703=EDGE_LOOP('',(#1477));
#704=EDGE_LOOP('',(#1478));
#705=EDGE_LOOP('',(#1479));
#706=EDGE_LOOP('',(#1480));
#707=EDGE_LOOP('',(#1481,#1482,#1483,#1484));
#708=EDGE_LOOP('',(#1485,#1486,#1487,#1488,#1489,#1490,#1491,#1492,#1493,
#1494,#1495,#1496));
#709=EDGE_LOOP('',(#1497,#1498,#1499,#1500));
#710=EDGE_LOOP('',(#1501,#1502,#1503,#1504,#1505,#1506,#1507,#1508,#1509,
#1510,#1511,#1512));
#711=EDGE_LOOP('',(#1513,#1514,#1515,#1516));
#712=EDGE_LOOP('',(#1517,#1518,#1519,#1520));
#713=EDGE_LOOP('',(#1521,#1522,#1523,#1524));
#714=EDGE_LOOP('',(#1525,#1526,#1527,#1528));
#715=EDGE_LOOP('',(#1529,#1530,#1531,#1532));
#716=EDGE_LOOP('',(#1533,#1534,#1535,#1536));
#717=EDGE_LOOP('',(#1537,#1538,#1539,#1540));
#718=EDGE_LOOP('',(#1541,#1542,#1543,#1544));
#719=EDGE_LOOP('',(#1545,#1546,#1547,#1548));
#720=EDGE_LOOP('',(#1549,#1550,#1551,#1552));
#721=EDGE_LOOP('',(#1553,#1554,#1555,#1556));
#722=EDGE_LOOP('',(#1557,#1558,#1559,#1560));
#723=EDGE_LOOP('',(#1561,#1562,#1563,#1564));
#724=EDGE_LOOP('',(#1565));
#725=EDGE_LOOP('',(#1566,#1567,#1568,#1569));
#726=EDGE_LOOP('',(#1570));
#727=EDGE_LOOP('',(#1571,#1572,#1573,#1574));
#728=EDGE_LOOP('',(#1575));
#729=EDGE_LOOP('',(#1576));
#730=EDGE_LOOP('',(#1577,#1578,#1579,#1580));
#731=EDGE_LOOP('',(#1581,#1582,#1583,#1584,#1585,#1586,#1587,#1588,#1589,
#1590));
#732=EDGE_LOOP('',(#1591));
#733=EDGE_LOOP('',(#1592,#1593,#1594,#1595));
#734=EDGE_LOOP('',(#1596,#1597,#1598,#1599,#1600,#1601,#1602,#1603,#1604,
#1605));
#735=EDGE_LOOP('',(#1606));
#736=EDGE_LOOP('',(#1607,#1608,#1609,#1610,#1611,#1612,#1613,#1614));
#737=EDGE_LOOP('',(#1615,#1616,#1617,#1618,#1619,#1620,#1621,#1622));
#738=EDGE_LOOP('',(#1623,#1624,#1625,#1626));
#739=EDGE_LOOP('',(#1627,#1628,#1629,#1630,#1631,#1632));
#740=EDGE_LOOP('',(#1633));
#741=EDGE_LOOP('',(#1634,#1635,#1636,#1637,#1638,#1639));
#742=EDGE_LOOP('',(#1640));
#743=EDGE_LOOP('',(#1641,#1642,#1643,#1644));
#744=EDGE_LOOP('',(#1645,#1646,#1647,#1648));
#745=EDGE_LOOP('',(#1649,#1650,#1651,#1652));
#746=EDGE_LOOP('',(#1653,#1654,#1655,#1656));
#747=EDGE_LOOP('',(#1657,#1658,#1659,#1660));
#748=EDGE_LOOP('',(#1661,#1662,#1663,#1664));
#749=EDGE_LOOP('',(#1665,#1666,#1667,#1668,#1669));
#750=EDGE_LOOP('',(#1670,#1671,#1672,#1673,#1674));
#751=EDGE_LOOP('',(#1675));
#752=EDGE_LOOP('',(#1676));
#753=CIRCLE('',#1879,7.5);
#754=CIRCLE('',#1880,1.5);
#755=CIRCLE('',#1881,6.);
#756=CIRCLE('',#1883,7.49999999999999);
#757=CIRCLE('',#1884,7.49999999999999);
#758=CIRCLE('',#1885,3.);
#759=CIRCLE('',#1886,4.49999999999999);
#760=CIRCLE('',#1888,15.);
#761=CIRCLE('',#1889,15.);
#762=CIRCLE('',#1891,7.5);
#763=CIRCLE('',#1893,7.5);
#764=CIRCLE('',#1894,7.49999999999999);
#765=CIRCLE('',#1895,7.49999999999999);
#766=CIRCLE('',#1905,15.);
#767=CIRCLE('',#1906,15.);
#768=CIRCLE('',#1907,13.5);
#769=CIRCLE('',#1909,24.);
#770=CIRCLE('',#1910,24.);
#771=CIRCLE('',#1911,22.5);
#772=CIRCLE('',#1913,24.);
#773=CIRCLE('',#1914,22.5);
#774=CIRCLE('',#1918,7.5);
#775=CIRCLE('',#1919,7.5);
#776=CIRCLE('',#1921,15.);
#777=CIRCLE('',#1927,4.5);
#778=CIRCLE('',#1928,4.5);
#779=CIRCLE('',#1930,3.75);
#780=CIRCLE('',#1931,3.75);
#781=CIRCLE('',#1933,3.75);
#782=CIRCLE('',#1934,3.75);
#783=CIRCLE('',#1936,7.50000000000001);
#784=CIRCLE('',#1937,7.50000000000001);
#785=CIRCLE('',#1951,4.50000000000001);
#786=CIRCLE('',#1952,4.50000000000001);
#787=CIRCLE('',#1954,7.50000000000002);
#788=CIRCLE('',#1955,7.50000000000002);
#789=CIRCLE('',#1957,33.7500000000001);
#790=CIRCLE('',#1958,33.7500000000001);
#791=CIRCLE('',#1963,6.);
#792=CIRCLE('',#1964,6.);
#793=CIRCLE('',#1966,4.5);
#794=CIRCLE('',#1967,4.5);
#795=CIRCLE('',#1969,11.25);
#796=CIRCLE('',#1970,11.25);
#797=CIRCLE('',#1972,11.25);
#798=CIRCLE('',#1973,6.);
#799=CIRCLE('',#1975,11.25);
#800=CIRCLE('',#1976,6.);
#801=CIRCLE('',#1985,4.5);
#802=CIRCLE('',#1986,4.5);
#803=CIRCLE('',#1988,4.5);
#804=CIRCLE('',#1989,4.5);
#805=CIRCLE('',#1991,4.5);
#806=CIRCLE('',#1992,4.5);
#807=CIRCLE('',#1994,4.5);
#808=CIRCLE('',#1995,4.5);
#809=CIRCLE('',#1997,3.75);
#810=CIRCLE('',#1998,3.75);
#811=CIRCLE('',#2000,3.75);
#812=CIRCLE('',#2001,3.75);
#813=CIRCLE('',#2018,4.50000000000001);
#814=CIRCLE('',#2019,4.50000000000001);
#815=CIRCLE('',#2021,4.50000000000001);
#816=CIRCLE('',#2022,4.50000000000001);
#817=CIRCLE('',#2024,4.50000000000002);
#818=CIRCLE('',#2025,4.50000000000002);
#819=CIRCLE('',#2027,4.50000000000001);
#820=CIRCLE('',#2028,4.50000000000001);
#821=CIRCLE('',#2035,3.00000000000001);
#822=CIRCLE('',#2036,3.00000000000001);
#823=CIRCLE('',#2039,3.00000000000001);
#824=CIRCLE('',#2040,3.00000000000001);
#825=CIRCLE('',#2045,3.00000000000001);
#826=CIRCLE('',#2046,3.00000000000001);
#827=CIRCLE('',#2048,3.00000000000001);
#828=CIRCLE('',#2049,3.00000000000001);
#829=CIRCLE('',#2057,4.50000000000002);
#830=CIRCLE('',#2058,3.54);
#831=CIRCLE('',#2060,4.50000000000002);
#832=CIRCLE('',#2061,4.50000000000002);
#833=CIRCLE('',#2062,3.54000000000001);
#834=VERTEX_POINT('',#2621);
#835=VERTEX_POINT('',#2623);
#836=VERTEX_POINT('',#2627);
#837=VERTEX_POINT('',#2628);
#838=VERTEX_POINT('',#2631);
#839=VERTEX_POINT('',#2635);
#840=VERTEX_POINT('',#2637);
#841=VERTEX_POINT('',#2641);
#842=VERTEX_POINT('',#2645);
#843=VERTEX_POINT('',#2648);
#844=VERTEX_POINT('',#2649);
#845=VERTEX_POINT('',#2651);
#846=VERTEX_POINT('',#2653);
#847=VERTEX_POINT('',#2667);
#848=VERTEX_POINT('',#2668);
#849=VERTEX_POINT('',#2671);
#850=VERTEX_POINT('',#2675);
#851=VERTEX_POINT('',#2676);
#852=VERTEX_POINT('',#2679);
#853=VERTEX_POINT('',#2683);
#854=VERTEX_POINT('',#2685);
#855=VERTEX_POINT('',#2689);
#856=VERTEX_POINT('',#2690);
#857=VERTEX_POINT('',#2709);
#858=VERTEX_POINT('',#2711);
#859=VERTEX_POINT('',#2769);
#860=VERTEX_POINT('',#2771);
#861=VERTEX_POINT('',#2775);
#862=VERTEX_POINT('',#2783);
#863=VERTEX_POINT('',#2785);
#864=VERTEX_POINT('',#2789);
#865=VERTEX_POINT('',#2791);
#866=VERTEX_POINT('',#2795);
#867=VERTEX_POINT('',#2797);
#868=VERTEX_POINT('',#2801);
#869=VERTEX_POINT('',#2803);
#870=VERTEX_POINT('',#2807);
#871=VERTEX_POINT('',#2808);
#872=VERTEX_POINT('',#2810);
#873=VERTEX_POINT('',#2812);
#874=VERTEX_POINT('',#2814);
#875=VERTEX_POINT('',#2816);
#876=VERTEX_POINT('',#2820);
#877=VERTEX_POINT('',#2821);
#878=VERTEX_POINT('',#2823);
#879=VERTEX_POINT('',#2825);
#880=VERTEX_POINT('',#2827);
#881=VERTEX_POINT('',#2829);
#882=VERTEX_POINT('',#2849);
#883=VERTEX_POINT('',#2851);
#884=VERTEX_POINT('',#2855);
#885=VERTEX_POINT('',#2857);
#886=VERTEX_POINT('',#2861);
#887=VERTEX_POINT('',#2863);
#888=VERTEX_POINT('',#2870);
#889=VERTEX_POINT('',#2871);
#890=VERTEX_POINT('',#2873);
#891=VERTEX_POINT('',#2875);
#892=VERTEX_POINT('',#2879);
#893=VERTEX_POINT('',#2881);
#894=VERTEX_POINT('',#2885);
#895=VERTEX_POINT('',#2886);
#896=VERTEX_POINT('',#2888);
#897=VERTEX_POINT('',#2890);
#898=VERTEX_POINT('',#2894);
#899=VERTEX_POINT('',#2895);
#900=VERTEX_POINT('',#2899);
#901=VERTEX_POINT('',#2900);
#902=VERTEX_POINT('',#2905);
#903=VERTEX_POINT('',#2906);
#904=VERTEX_POINT('',#2910);
#905=VERTEX_POINT('',#2912);
#906=VERTEX_POINT('',#2927);
#907=VERTEX_POINT('',#2929);
#908=VERTEX_POINT('',#2933);
#909=VERTEX_POINT('',#2935);
#910=VERTEX_POINT('',#2939);
#911=VERTEX_POINT('',#2941);
#912=VERTEX_POINT('',#2945);
#913=VERTEX_POINT('',#2947);
#914=VERTEX_POINT('',#2951);
#915=VERTEX_POINT('',#2953);
#916=VERTEX_POINT('',#2957);
#917=VERTEX_POINT('',#2959);
#918=VERTEX_POINT('',#2963);
#919=VERTEX_POINT('',#2964);
#920=VERTEX_POINT('',#2966);
#921=VERTEX_POINT('',#2968);
#922=VERTEX_POINT('',#2972);
#923=VERTEX_POINT('',#2973);
#924=VERTEX_POINT('',#2975);
#925=VERTEX_POINT('',#2977);
#926=VERTEX_POINT('',#2981);
#927=VERTEX_POINT('',#2982);
#928=VERTEX_POINT('',#2984);
#929=VERTEX_POINT('',#2986);
#930=VERTEX_POINT('',#2990);
#931=VERTEX_POINT('',#2992);
#932=VERTEX_POINT('',#2996);
#933=VERTEX_POINT('',#2998);
#934=VERTEX_POINT('',#3001);
#935=VERTEX_POINT('',#3003);
#936=VERTEX_POINT('',#3006);
#937=VERTEX_POINT('',#3010);
#938=VERTEX_POINT('',#3014);
#939=VERTEX_POINT('',#3017);
#940=VERTEX_POINT('',#3019);
#941=VERTEX_POINT('',#3022);
#942=VERTEX_POINT('',#3038);
#943=VERTEX_POINT('',#3040);
#944=VERTEX_POINT('',#3044);
#945=VERTEX_POINT('',#3046);
#946=VERTEX_POINT('',#3050);
#947=VERTEX_POINT('',#3052);
#948=VERTEX_POINT('',#3056);
#949=VERTEX_POINT('',#3058);
#950=VERTEX_POINT('',#3062);
#951=VERTEX_POINT('',#3063);
#952=VERTEX_POINT('',#3065);
#953=VERTEX_POINT('',#3067);
#954=VERTEX_POINT('',#3071);
#955=VERTEX_POINT('',#3072);
#956=VERTEX_POINT('',#3074);
#957=VERTEX_POINT('',#3076);
#958=VERTEX_POINT('',#3080);
#959=VERTEX_POINT('',#3081);
#960=VERTEX_POINT('',#3083);
#961=VERTEX_POINT('',#3085);
#962=VERTEX_POINT('',#3089);
#963=VERTEX_POINT('',#3090);
#964=VERTEX_POINT('',#3092);
#965=VERTEX_POINT('',#3094);
#966=VERTEX_POINT('',#3101);
#967=VERTEX_POINT('',#3104);
#968=VERTEX_POINT('',#3111);
#969=VERTEX_POINT('',#3112);
#970=VERTEX_POINT('',#3114);
#971=VERTEX_POINT('',#3117);
#972=VERTEX_POINT('',#3121);
#973=VERTEX_POINT('',#3122);
#974=VERTEX_POINT('',#3125);
#975=VERTEX_POINT('',#3127);
#976=VERTEX_POINT('',#3131);
#977=VERTEX_POINT('',#3133);
#978=VERTEX_POINT('',#3135);
#979=VERTEX_POINT('',#3137);
#980=VERTEX_POINT('',#3141);
#981=VERTEX_POINT('',#3142);
#982=VERTEX_POINT('',#3161);
#983=VERTEX_POINT('',#3163);
#984=VERTEX_POINT('',#3167);
#985=VERTEX_POINT('',#3168);
#986=VERTEX_POINT('',#3171);
#987=EDGE_CURVE('',#834,#834,#753,.T.);
#988=EDGE_CURVE('',#834,#835,#754,.T.);
#989=EDGE_CURVE('',#835,#835,#755,.T.);
#990=EDGE_CURVE('',#836,#837,#756,.T.);
#991=EDGE_CURVE('',#837,#836,#757,.T.);
#992=EDGE_CURVE('',#837,#838,#758,.T.);
#993=EDGE_CURVE('',#838,#838,#759,.T.);
#994=EDGE_CURVE('',#839,#839,#760,.T.);
#995=EDGE_CURVE('',#839,#840,#188,.T.);
#996=EDGE_CURVE('',#840,#840,#761,.T.);
#997=EDGE_CURVE('',#841,#841,#762,.T.);
#998=EDGE_CURVE('',#841,#834,#189,.T.);
#999=EDGE_CURVE('',#836,#842,#190,.T.);
#1000=EDGE_CURVE('',#842,#842,#763,.T.);
#1001=EDGE_CURVE('',#843,#844,#764,.T.);
#1002=EDGE_CURVE('',#843,#845,#191,.T.);
#1003=EDGE_CURVE('',#845,#846,#765,.T.);
#1004=EDGE_CURVE('',#846,#844,#192,.T.);
#1005=EDGE_CURVE('',#846,#845,#193,.T.);
#1006=EDGE_CURVE('',#844,#843,#194,.T.);
#1007=EDGE_CURVE('',#847,#848,#766,.T.);
#1008=EDGE_CURVE('',#848,#847,#767,.T.);
#1009=EDGE_CURVE('',#848,#849,#195,.T.);
#1010=EDGE_CURVE('',#849,#849,#768,.T.);
#1011=EDGE_CURVE('',#850,#851,#769,.T.);
#1012=EDGE_CURVE('',#851,#850,#770,.T.);
#1013=EDGE_CURVE('',#851,#852,#196,.T.);
#1014=EDGE_CURVE('',#852,#852,#771,.T.);
#1015=EDGE_CURVE('',#853,#853,#772,.T.);
#1016=EDGE_CURVE('',#853,#854,#197,.T.);
#1017=EDGE_CURVE('',#854,#854,#773,.T.);
#1018=EDGE_CURVE('',#855,#856,#47,.T.);
#1019=EDGE_CURVE('',#856,#857,#198,.T.);
#1020=EDGE_CURVE('',#857,#858,#48,.T.);
#1021=EDGE_CURVE('',#858,#857,#49,.T.);
#1022=EDGE_CURVE('',#856,#855,#50,.T.);
#1023=EDGE_CURVE('',#850,#853,#199,.T.);
#1024=EDGE_CURVE('',#859,#859,#774,.T.);
#1025=EDGE_CURVE('',#859,#860,#200,.T.);
#1026=EDGE_CURVE('',#860,#860,#775,.T.);
#1027=EDGE_CURVE('',#847,#861,#201,.T.);
#1028=EDGE_CURVE('',#861,#861,#776,.T.);
#1029=EDGE_CURVE('',#862,#862,#777,.T.);
#1030=EDGE_CURVE('',#862,#863,#202,.T.);
#1031=EDGE_CURVE('',#863,#863,#778,.T.);
#1032=EDGE_CURVE('',#864,#864,#779,.T.);
#1033=EDGE_CURVE('',#864,#865,#203,.T.);
#1034=EDGE_CURVE('',#865,#865,#780,.T.);
#1035=EDGE_CURVE('',#866,#866,#781,.T.);
#1036=EDGE_CURVE('',#866,#867,#204,.T.);
#1037=EDGE_CURVE('',#867,#867,#782,.T.);
#1038=EDGE_CURVE('',#868,#868,#783,.T.);
#1039=EDGE_CURVE('',#868,#869,#205,.T.);
#1040=EDGE_CURVE('',#869,#869,#784,.T.);
#1041=EDGE_CURVE('',#870,#871,#206,.T.);
#1042=EDGE_CURVE('',#871,#872,#207,.T.);
#1043=EDGE_CURVE('',#872,#873,#208,.T.);
#1044=EDGE_CURVE('',#873,#874,#209,.T.);
#1045=EDGE_CURVE('',#874,#875,#210,.T.);
#1046=EDGE_CURVE('',#875,#870,#211,.T.);
#1047=EDGE_CURVE('',#876,#877,#212,.T.);
#1048=EDGE_CURVE('',#876,#878,#213,.T.);
#1049=EDGE_CURVE('',#879,#878,#214,.T.);
#1050=EDGE_CURVE('',#879,#880,#215,.T.);
#1051=EDGE_CURVE('',#881,#880,#216,.T.);
#1052=EDGE_CURVE('',#877,#881,#217,.T.);
#1053=EDGE_CURVE('',#872,#876,#218,.T.);
#1054=EDGE_CURVE('',#873,#877,#219,.T.);
#1055=EDGE_CURVE('',#874,#881,#220,.T.);
#1056=EDGE_CURVE('',#880,#875,#221,.T.);
#1057=EDGE_CURVE('',#878,#871,#222,.T.);
#1058=EDGE_CURVE('',#870,#879,#223,.T.);
#1059=EDGE_CURVE('',#882,#882,#785,.T.);
#1060=EDGE_CURVE('',#882,#883,#224,.T.);
#1061=EDGE_CURVE('',#883,#883,#786,.T.);
#1062=EDGE_CURVE('',#884,#884,#787,.T.);
#1063=EDGE_CURVE('',#884,#885,#225,.T.);
#1064=EDGE_CURVE('',#885,#885,#788,.T.);
#1065=EDGE_CURVE('',#886,#886,#789,.T.);
#1066=EDGE_CURVE('',#886,#887,#226,.T.);
#1067=EDGE_CURVE('',#887,#887,#790,.T.);
#1068=EDGE_CURVE('',#888,#889,#791,.T.);
#1069=EDGE_CURVE('',#889,#890,#227,.T.);
#1070=EDGE_CURVE('',#891,#890,#792,.T.);
#1071=EDGE_CURVE('',#888,#891,#228,.T.);
#1072=EDGE_CURVE('',#892,#892,#793,.T.);
#1073=EDGE_CURVE('',#892,#893,#229,.T.);
#1074=EDGE_CURVE('',#893,#893,#794,.T.);
#1075=EDGE_CURVE('',#894,#895,#795,.T.);
#1076=EDGE_CURVE('',#894,#896,#230,.T.);
#1077=EDGE_CURVE('',#896,#897,#796,.T.);
#1078=EDGE_CURVE('',#895,#897,#231,.T.);
#1079=EDGE_CURVE('',#898,#899,#797,.T.);
#1080=EDGE_CURVE('',#899,#894,#232,.T.);
#1081=EDGE_CURVE('',#895,#898,#233,.T.);
#1082=EDGE_CURVE('',#900,#901,#798,.T.);
#1083=EDGE_CURVE('',#889,#900,#234,.T.);
#1084=EDGE_CURVE('',#901,#888,#235,.T.);
#1085=EDGE_CURVE('',#902,#903,#799,.T.);
#1086=EDGE_CURVE('',#897,#902,#236,.T.);
#1087=EDGE_CURVE('',#903,#896,#237,.T.);
#1088=EDGE_CURVE('',#890,#904,#238,.T.);
#1089=EDGE_CURVE('',#904,#905,#800,.T.);
#1090=EDGE_CURVE('',#905,#891,#239,.T.);
#1091=EDGE_CURVE('',#899,#903,#240,.T.);
#1092=EDGE_CURVE('',#898,#902,#241,.T.);
#1093=EDGE_CURVE('',#900,#904,#242,.T.);
#1094=EDGE_CURVE('',#901,#905,#243,.T.);
#1095=EDGE_CURVE('',#906,#906,#801,.T.);
#1096=EDGE_CURVE('',#906,#907,#244,.T.);
#1097=EDGE_CURVE('',#907,#907,#802,.T.);
#1098=EDGE_CURVE('',#908,#908,#803,.T.);
#1099=EDGE_CURVE('',#908,#909,#245,.T.);
#1100=EDGE_CURVE('',#909,#909,#804,.T.);
#1101=EDGE_CURVE('',#910,#910,#805,.T.);
#1102=EDGE_CURVE('',#910,#911,#246,.T.);
#1103=EDGE_CURVE('',#911,#911,#806,.T.);
#1104=EDGE_CURVE('',#912,#912,#807,.T.);
#1105=EDGE_CURVE('',#912,#913,#247,.T.);
#1106=EDGE_CURVE('',#913,#913,#808,.T.);
#1107=EDGE_CURVE('',#914,#914,#809,.T.);
#1108=EDGE_CURVE('',#914,#915,#248,.T.);
#1109=EDGE_CURVE('',#915,#915,#810,.T.);
#1110=EDGE_CURVE('',#916,#916,#811,.T.);
#1111=EDGE_CURVE('',#916,#917,#249,.T.);
#1112=EDGE_CURVE('',#917,#917,#812,.T.);
#1113=EDGE_CURVE('',#918,#919,#250,.T.);
#1114=EDGE_CURVE('',#919,#920,#251,.T.);
#1115=EDGE_CURVE('',#920,#921,#252,.T.);
#1116=EDGE_CURVE('',#921,#918,#253,.T.);
#1117=EDGE_CURVE('',#922,#923,#254,.T.);
#1118=EDGE_CURVE('',#923,#924,#255,.T.);
#1119=EDGE_CURVE('',#924,#925,#256,.T.);
#1120=EDGE_CURVE('',#925,#922,#257,.T.);
#1121=EDGE_CURVE('',#926,#927,#258,.T.);
#1122=EDGE_CURVE('',#928,#926,#259,.T.);
#1123=EDGE_CURVE('',#929,#928,#260,.T.);
#1124=EDGE_CURVE('',#927,#929,#261,.T.);
#1125=EDGE_CURVE('',#930,#927,#262,.T.);
#1126=EDGE_CURVE('',#931,#930,#263,.T.);
#1127=EDGE_CURVE('',#931,#926,#264,.T.);
#1128=EDGE_CURVE('',#932,#929,#265,.T.);
#1129=EDGE_CURVE('',#933,#932,#266,.T.);
#1130=EDGE_CURVE('',#933,#918,#267,.T.);
#1131=EDGE_CURVE('',#934,#921,#268,.T.);
#1132=EDGE_CURVE('',#935,#934,#269,.T.);
#1133=EDGE_CURVE('',#935,#924,#270,.T.);
#1134=EDGE_CURVE('',#936,#923,#271,.T.);
#1135=EDGE_CURVE('',#930,#936,#272,.T.);
#1136=EDGE_CURVE('',#937,#928,#273,.T.);
#1137=EDGE_CURVE('',#932,#937,#274,.T.);
#1138=EDGE_CURVE('',#938,#931,#275,.T.);
#1139=EDGE_CURVE('',#938,#922,#276,.T.);
#1140=EDGE_CURVE('',#939,#925,#277,.T.);
#1141=EDGE_CURVE('',#940,#939,#278,.T.);
#1142=EDGE_CURVE('',#940,#920,#279,.T.);
#1143=EDGE_CURVE('',#941,#919,#280,.T.);
#1144=EDGE_CURVE('',#937,#941,#281,.T.);
#1145=EDGE_CURVE('',#940,#934,#282,.T.);
#1146=EDGE_CURVE('',#935,#939,#283,.T.);
#1147=EDGE_CURVE('',#933,#941,#284,.T.);
#1148=EDGE_CURVE('',#938,#936,#285,.T.);
#1149=EDGE_CURVE('',#942,#942,#813,.T.);
#1150=EDGE_CURVE('',#942,#943,#286,.T.);
#1151=EDGE_CURVE('',#943,#943,#814,.T.);
#1152=EDGE_CURVE('',#944,#944,#815,.T.);
#1153=EDGE_CURVE('',#944,#945,#287,.T.);
#1154=EDGE_CURVE('',#945,#945,#816,.T.);
#1155=EDGE_CURVE('',#946,#946,#817,.T.);
#1156=EDGE_CURVE('',#946,#947,#288,.T.);
#1157=EDGE_CURVE('',#947,#947,#818,.T.);
#1158=EDGE_CURVE('',#948,#948,#819,.T.);
#1159=EDGE_CURVE('',#948,#949,#289,.T.);
#1160=EDGE_CURVE('',#949,#949,#820,.T.);
#1161=EDGE_CURVE('',#950,#951,#290,.T.);
#1162=EDGE_CURVE('',#951,#952,#291,.T.);
#1163=EDGE_CURVE('',#953,#952,#292,.T.);
#1164=EDGE_CURVE('',#953,#950,#293,.T.);
#1165=EDGE_CURVE('',#954,#955,#294,.T.);
#1166=EDGE_CURVE('',#954,#956,#295,.T.);
#1167=EDGE_CURVE('',#956,#957,#296,.T.);
#1168=EDGE_CURVE('',#957,#955,#297,.T.);
#1169=EDGE_CURVE('',#958,#959,#298,.T.);
#1170=EDGE_CURVE('',#958,#960,#299,.T.);
#1171=EDGE_CURVE('',#960,#961,#300,.T.);
#1172=EDGE_CURVE('',#961,#959,#301,.T.);
#1173=EDGE_CURVE('',#962,#963,#302,.T.);
#1174=EDGE_CURVE('',#964,#962,#303,.T.);
#1175=EDGE_CURVE('',#965,#964,#304,.T.);
#1176=EDGE_CURVE('',#963,#965,#305,.T.);
#1177=EDGE_CURVE('',#961,#963,#306,.T.);
#1178=EDGE_CURVE('',#960,#962,#307,.T.);
#1179=EDGE_CURVE('',#966,#954,#308,.T.);
#1180=EDGE_CURVE('',#966,#951,#821,.T.);
#1181=EDGE_CURVE('',#950,#967,#822,.T.);
#1182=EDGE_CURVE('',#967,#959,#309,.T.);
#1183=EDGE_CURVE('',#956,#965,#310,.T.);
#1184=EDGE_CURVE('',#957,#964,#311,.T.);
#1185=EDGE_CURVE('',#968,#969,#312,.T.);
#1186=EDGE_CURVE('',#968,#970,#823,.T.);
#1187=EDGE_CURVE('',#970,#955,#313,.T.);
#1188=EDGE_CURVE('',#971,#958,#314,.T.);
#1189=EDGE_CURVE('',#971,#969,#824,.T.);
#1190=EDGE_CURVE('',#972,#973,#315,.T.);
#1191=EDGE_CURVE('',#973,#971,#316,.T.);
#1192=EDGE_CURVE('',#967,#974,#317,.T.);
#1193=EDGE_CURVE('',#975,#974,#318,.T.);
#1194=EDGE_CURVE('',#972,#975,#319,.T.);
#1195=EDGE_CURVE('',#970,#976,#320,.T.);
#1196=EDGE_CURVE('',#977,#976,#321,.T.);
#1197=EDGE_CURVE('',#978,#977,#322,.T.);
#1198=EDGE_CURVE('',#978,#979,#323,.T.);
#1199=EDGE_CURVE('',#979,#966,#324,.T.);
#1200=EDGE_CURVE('',#980,#981,#325,.T.);
#1201=EDGE_CURVE('',#980,#968,#326,.T.);
#1202=EDGE_CURVE('',#969,#981,#327,.T.);
#1203=EDGE_CURVE('',#952,#979,#825,.T.);
#1204=EDGE_CURVE('',#975,#978,#328,.T.);
#1205=EDGE_CURVE('',#974,#953,#826,.T.);
#1206=EDGE_CURVE('',#976,#980,#827,.T.);
#1207=EDGE_CURVE('',#981,#973,#828,.T.);
#1208=EDGE_CURVE('',#977,#972,#329,.T.);
#1209=EDGE_CURVE('',#982,#982,#829,.T.);
#1210=EDGE_CURVE('',#982,#983,#330,.T.);
#1211=EDGE_CURVE('',#983,#983,#830,.T.);
#1212=EDGE_CURVE('',#984,#985,#831,.T.);
#1213=EDGE_CURVE('',#985,#984,#832,.T.);
#1214=EDGE_CURVE('',#985,#986,#331,.T.);
#1215=EDGE_CURVE('',#986,#986,#833,.T.);
#1216=EDGE_CURVE('',#984,#982,#332,.T.);
#1217=ORIENTED_EDGE('',*,*,#987,.F.);
#1218=ORIENTED_EDGE('',*,*,#988,.T.);
#1219=ORIENTED_EDGE('',*,*,#989,.F.);
#1220=ORIENTED_EDGE('',*,*,#988,.F.);
#1221=ORIENTED_EDGE('',*,*,#990,.F.);
#1222=ORIENTED_EDGE('',*,*,#991,.F.);
#1223=ORIENTED_EDGE('',*,*,#992,.T.);
#1224=ORIENTED_EDGE('',*,*,#993,.F.);
#1225=ORIENTED_EDGE('',*,*,#992,.F.);
#1226=ORIENTED_EDGE('',*,*,#994,.F.);
#1227=ORIENTED_EDGE('',*,*,#995,.T.);
#1228=ORIENTED_EDGE('',*,*,#996,.T.);
#1229=ORIENTED_EDGE('',*,*,#995,.F.);
#1230=ORIENTED_EDGE('',*,*,#997,.F.);
#1231=ORIENTED_EDGE('',*,*,#998,.T.);
#1232=ORIENTED_EDGE('',*,*,#987,.T.);
#1233=ORIENTED_EDGE('',*,*,#998,.F.);
#1234=ORIENTED_EDGE('',*,*,#990,.T.);
#1235=ORIENTED_EDGE('',*,*,#991,.T.);
#1236=ORIENTED_EDGE('',*,*,#999,.T.);
#1237=ORIENTED_EDGE('',*,*,#1000,.T.);
#1238=ORIENTED_EDGE('',*,*,#999,.F.);
#1239=ORIENTED_EDGE('',*,*,#1001,.F.);
#1240=ORIENTED_EDGE('',*,*,#1002,.T.);
#1241=ORIENTED_EDGE('',*,*,#1003,.T.);
#1242=ORIENTED_EDGE('',*,*,#1004,.T.);
#1243=ORIENTED_EDGE('',*,*,#989,.T.);
#1244=ORIENTED_EDGE('',*,*,#996,.F.);
#1245=ORIENTED_EDGE('',*,*,#997,.T.);
#1246=ORIENTED_EDGE('',*,*,#994,.T.);
#1247=ORIENTED_EDGE('',*,*,#1000,.F.);
#1248=ORIENTED_EDGE('',*,*,#993,.T.);
#1249=ORIENTED_EDGE('',*,*,#1005,.T.);
#1250=ORIENTED_EDGE('',*,*,#1002,.F.);
#1251=ORIENTED_EDGE('',*,*,#1006,.F.);
#1252=ORIENTED_EDGE('',*,*,#1004,.F.);
#1253=ORIENTED_EDGE('',*,*,#1006,.T.);
#1254=ORIENTED_EDGE('',*,*,#1001,.T.);
#1255=ORIENTED_EDGE('',*,*,#1005,.F.);
#1256=ORIENTED_EDGE('',*,*,#1003,.F.);
#1257=ORIENTED_EDGE('',*,*,#1007,.F.);
#1258=ORIENTED_EDGE('',*,*,#1008,.F.);
#1259=ORIENTED_EDGE('',*,*,#1009,.T.);
#1260=ORIENTED_EDGE('',*,*,#1010,.F.);
#1261=ORIENTED_EDGE('',*,*,#1009,.F.);
#1262=ORIENTED_EDGE('',*,*,#1011,.F.);
#1263=ORIENTED_EDGE('',*,*,#1012,.F.);
#1264=ORIENTED_EDGE('',*,*,#1013,.T.);
#1265=ORIENTED_EDGE('',*,*,#1014,.F.);
#1266=ORIENTED_EDGE('',*,*,#1013,.F.);
#1267=ORIENTED_EDGE('',*,*,#1015,.F.);
#1268=ORIENTED_EDGE('',*,*,#1016,.T.);
#1269=ORIENTED_EDGE('',*,*,#1017,.F.);
#1270=ORIENTED_EDGE('',*,*,#1016,.F.);
#1271=ORIENTED_EDGE('',*,*,#1018,.T.);
#1272=ORIENTED_EDGE('',*,*,#1019,.T.);
#1273=ORIENTED_EDGE('',*,*,#1020,.T.);
#1274=ORIENTED_EDGE('',*,*,#1021,.T.);
#1275=ORIENTED_EDGE('',*,*,#1019,.F.);
#1276=ORIENTED_EDGE('',*,*,#1022,.T.);
#1277=ORIENTED_EDGE('',*,*,#1011,.T.);
#1278=ORIENTED_EDGE('',*,*,#1012,.T.);
#1279=ORIENTED_EDGE('',*,*,#1023,.T.);
#1280=ORIENTED_EDGE('',*,*,#1015,.T.);
#1281=ORIENTED_EDGE('',*,*,#1023,.F.);
#1282=ORIENTED_EDGE('',*,*,#1024,.F.);
#1283=ORIENTED_EDGE('',*,*,#1025,.T.);
#1284=ORIENTED_EDGE('',*,*,#1026,.T.);
#1285=ORIENTED_EDGE('',*,*,#1025,.F.);
#1286=ORIENTED_EDGE('',*,*,#1021,.F.);
#1287=ORIENTED_EDGE('',*,*,#1020,.F.);
#1288=ORIENTED_EDGE('',*,*,#1007,.T.);
#1289=ORIENTED_EDGE('',*,*,#1008,.T.);
#1290=ORIENTED_EDGE('',*,*,#1027,.T.);
#1291=ORIENTED_EDGE('',*,*,#1028,.T.);
#1292=ORIENTED_EDGE('',*,*,#1027,.F.);
#1293=ORIENTED_EDGE('',*,*,#1018,.F.);
#1294=ORIENTED_EDGE('',*,*,#1022,.F.);
#1295=ORIENTED_EDGE('',*,*,#1017,.T.);
#1296=ORIENTED_EDGE('',*,*,#1026,.F.);
#1297=ORIENTED_EDGE('',*,*,#1014,.T.);
#1298=ORIENTED_EDGE('',*,*,#1028,.F.);
#1299=ORIENTED_EDGE('',*,*,#1010,.T.);
#1300=ORIENTED_EDGE('',*,*,#1024,.T.);
#1301=ORIENTED_EDGE('',*,*,#1029,.F.);
#1302=ORIENTED_EDGE('',*,*,#1030,.T.);
#1303=ORIENTED_EDGE('',*,*,#1031,.T.);
#1304=ORIENTED_EDGE('',*,*,#1030,.F.);
#1305=ORIENTED_EDGE('',*,*,#1032,.F.);
#1306=ORIENTED_EDGE('',*,*,#1033,.T.);
#1307=ORIENTED_EDGE('',*,*,#1034,.T.);
#1308=ORIENTED_EDGE('',*,*,#1033,.F.);
#1309=ORIENTED_EDGE('',*,*,#1035,.F.);
#1310=ORIENTED_EDGE('',*,*,#1036,.T.);
#1311=ORIENTED_EDGE('',*,*,#1037,.T.);
#1312=ORIENTED_EDGE('',*,*,#1036,.F.);
#1313=ORIENTED_EDGE('',*,*,#1038,.T.);
#1314=ORIENTED_EDGE('',*,*,#1039,.T.);
#1315=ORIENTED_EDGE('',*,*,#1040,.F.);
#1316=ORIENTED_EDGE('',*,*,#1039,.F.);
#1317=ORIENTED_EDGE('',*,*,#1041,.T.);
#1318=ORIENTED_EDGE('',*,*,#1042,.T.);
#1319=ORIENTED_EDGE('',*,*,#1043,.T.);
#1320=ORIENTED_EDGE('',*,*,#1044,.T.);
#1321=ORIENTED_EDGE('',*,*,#1045,.T.);
#1322=ORIENTED_EDGE('',*,*,#1046,.T.);
#1323=ORIENTED_EDGE('',*,*,#1038,.F.);
#1324=ORIENTED_EDGE('',*,*,#1047,.F.);
#1325=ORIENTED_EDGE('',*,*,#1048,.T.);
#1326=ORIENTED_EDGE('',*,*,#1049,.F.);
#1327=ORIENTED_EDGE('',*,*,#1050,.T.);
#1328=ORIENTED_EDGE('',*,*,#1051,.F.);
#1329=ORIENTED_EDGE('',*,*,#1052,.F.);
#1330=ORIENTED_EDGE('',*,*,#1040,.T.);
#1331=ORIENTED_EDGE('',*,*,#1043,.F.);
#1332=ORIENTED_EDGE('',*,*,#1053,.T.);
#1333=ORIENTED_EDGE('',*,*,#1047,.T.);
#1334=ORIENTED_EDGE('',*,*,#1054,.F.);
#1335=ORIENTED_EDGE('',*,*,#1052,.T.);
#1336=ORIENTED_EDGE('',*,*,#1055,.F.);
#1337=ORIENTED_EDGE('',*,*,#1044,.F.);
#1338=ORIENTED_EDGE('',*,*,#1054,.T.);
#1339=ORIENTED_EDGE('',*,*,#1031,.F.);
#1340=ORIENTED_EDGE('',*,*,#1034,.F.);
#1341=ORIENTED_EDGE('',*,*,#1037,.F.);
#1342=ORIENTED_EDGE('',*,*,#1051,.T.);
#1343=ORIENTED_EDGE('',*,*,#1056,.T.);
#1344=ORIENTED_EDGE('',*,*,#1045,.F.);
#1345=ORIENTED_EDGE('',*,*,#1055,.T.);
#1346=ORIENTED_EDGE('',*,*,#1049,.T.);
#1347=ORIENTED_EDGE('',*,*,#1057,.T.);
#1348=ORIENTED_EDGE('',*,*,#1041,.F.);
#1349=ORIENTED_EDGE('',*,*,#1058,.T.);
#1350=ORIENTED_EDGE('',*,*,#1042,.F.);
#1351=ORIENTED_EDGE('',*,*,#1057,.F.);
#1352=ORIENTED_EDGE('',*,*,#1048,.F.);
#1353=ORIENTED_EDGE('',*,*,#1053,.F.);
#1354=ORIENTED_EDGE('',*,*,#1046,.F.);
#1355=ORIENTED_EDGE('',*,*,#1056,.F.);
#1356=ORIENTED_EDGE('',*,*,#1050,.F.);
#1357=ORIENTED_EDGE('',*,*,#1058,.F.);
#1358=ORIENTED_EDGE('',*,*,#1035,.T.);
#1359=ORIENTED_EDGE('',*,*,#1032,.T.);
#1360=ORIENTED_EDGE('',*,*,#1029,.T.);
#1361=ORIENTED_EDGE('',*,*,#1059,.T.);
#1362=ORIENTED_EDGE('',*,*,#1060,.T.);
#1363=ORIENTED_EDGE('',*,*,#1061,.F.);
#1364=ORIENTED_EDGE('',*,*,#1060,.F.);
#1365=ORIENTED_EDGE('',*,*,#1062,.T.);
#1366=ORIENTED_EDGE('',*,*,#1063,.T.);
#1367=ORIENTED_EDGE('',*,*,#1064,.F.);
#1368=ORIENTED_EDGE('',*,*,#1063,.F.);
#1369=ORIENTED_EDGE('',*,*,#1065,.T.);
#1370=ORIENTED_EDGE('',*,*,#1066,.T.);
#1371=ORIENTED_EDGE('',*,*,#1067,.F.);
#1372=ORIENTED_EDGE('',*,*,#1066,.F.);
#1373=ORIENTED_EDGE('',*,*,#1067,.T.);
#1374=ORIENTED_EDGE('',*,*,#1059,.F.);
#1375=ORIENTED_EDGE('',*,*,#1062,.F.);
#1376=ORIENTED_EDGE('',*,*,#1065,.F.);
#1377=ORIENTED_EDGE('',*,*,#1061,.T.);
#1378=ORIENTED_EDGE('',*,*,#1064,.T.);
#1379=ORIENTED_EDGE('',*,*,#1068,.T.);
#1380=ORIENTED_EDGE('',*,*,#1069,.T.);
#1381=ORIENTED_EDGE('',*,*,#1070,.F.);
#1382=ORIENTED_EDGE('',*,*,#1071,.F.);
#1383=ORIENTED_EDGE('',*,*,#1072,.T.);
#1384=ORIENTED_EDGE('',*,*,#1073,.T.);
#1385=ORIENTED_EDGE('',*,*,#1074,.F.);
#1386=ORIENTED_EDGE('',*,*,#1073,.F.);
#1387=ORIENTED_EDGE('',*,*,#1075,.F.);
#1388=ORIENTED_EDGE('',*,*,#1076,.T.);
#1389=ORIENTED_EDGE('',*,*,#1077,.T.);
#1390=ORIENTED_EDGE('',*,*,#1078,.F.);
#1391=ORIENTED_EDGE('',*,*,#1079,.T.);
#1392=ORIENTED_EDGE('',*,*,#1080,.T.);
#1393=ORIENTED_EDGE('',*,*,#1075,.T.);
#1394=ORIENTED_EDGE('',*,*,#1081,.T.);
#1395=ORIENTED_EDGE('',*,*,#1082,.F.);
#1396=ORIENTED_EDGE('',*,*,#1083,.F.);
#1397=ORIENTED_EDGE('',*,*,#1068,.F.);
#1398=ORIENTED_EDGE('',*,*,#1084,.F.);
#1399=ORIENTED_EDGE('',*,*,#1072,.F.);
#1400=ORIENTED_EDGE('',*,*,#1085,.F.);
#1401=ORIENTED_EDGE('',*,*,#1086,.F.);
#1402=ORIENTED_EDGE('',*,*,#1077,.F.);
#1403=ORIENTED_EDGE('',*,*,#1087,.F.);
#1404=ORIENTED_EDGE('',*,*,#1088,.T.);
#1405=ORIENTED_EDGE('',*,*,#1089,.T.);
#1406=ORIENTED_EDGE('',*,*,#1090,.T.);
#1407=ORIENTED_EDGE('',*,*,#1070,.T.);
#1408=ORIENTED_EDGE('',*,*,#1074,.T.);
#1409=ORIENTED_EDGE('',*,*,#1085,.T.);
#1410=ORIENTED_EDGE('',*,*,#1091,.F.);
#1411=ORIENTED_EDGE('',*,*,#1079,.F.);
#1412=ORIENTED_EDGE('',*,*,#1092,.T.);
#1413=ORIENTED_EDGE('',*,*,#1087,.T.);
#1414=ORIENTED_EDGE('',*,*,#1076,.F.);
#1415=ORIENTED_EDGE('',*,*,#1080,.F.);
#1416=ORIENTED_EDGE('',*,*,#1091,.T.);
#1417=ORIENTED_EDGE('',*,*,#1086,.T.);
#1418=ORIENTED_EDGE('',*,*,#1092,.F.);
#1419=ORIENTED_EDGE('',*,*,#1081,.F.);
#1420=ORIENTED_EDGE('',*,*,#1078,.T.);
#1421=ORIENTED_EDGE('',*,*,#1089,.F.);
#1422=ORIENTED_EDGE('',*,*,#1093,.F.);
#1423=ORIENTED_EDGE('',*,*,#1082,.T.);
#1424=ORIENTED_EDGE('',*,*,#1094,.T.);
#1425=ORIENTED_EDGE('',*,*,#1090,.F.);
#1426=ORIENTED_EDGE('',*,*,#1094,.F.);
#1427=ORIENTED_EDGE('',*,*,#1084,.T.);
#1428=ORIENTED_EDGE('',*,*,#1071,.T.);
#1429=ORIENTED_EDGE('',*,*,#1088,.F.);
#1430=ORIENTED_EDGE('',*,*,#1069,.F.);
#1431=ORIENTED_EDGE('',*,*,#1083,.T.);
#1432=ORIENTED_EDGE('',*,*,#1093,.T.);
#1433=ORIENTED_EDGE('',*,*,#1095,.T.);
#1434=ORIENTED_EDGE('',*,*,#1096,.T.);
#1435=ORIENTED_EDGE('',*,*,#1097,.F.);
#1436=ORIENTED_EDGE('',*,*,#1096,.F.);
#1437=ORIENTED_EDGE('',*,*,#1098,.T.);
#1438=ORIENTED_EDGE('',*,*,#1099,.T.);
#1439=ORIENTED_EDGE('',*,*,#1100,.F.);
#1440=ORIENTED_EDGE('',*,*,#1099,.F.);
#1441=ORIENTED_EDGE('',*,*,#1101,.T.);
#1442=ORIENTED_EDGE('',*,*,#1102,.T.);
#1443=ORIENTED_EDGE('',*,*,#1103,.F.);
#1444=ORIENTED_EDGE('',*,*,#1102,.F.);
#1445=ORIENTED_EDGE('',*,*,#1104,.T.);
#1446=ORIENTED_EDGE('',*,*,#1105,.T.);
#1447=ORIENTED_EDGE('',*,*,#1106,.F.);
#1448=ORIENTED_EDGE('',*,*,#1105,.F.);
#1449=ORIENTED_EDGE('',*,*,#1107,.T.);
#1450=ORIENTED_EDGE('',*,*,#1108,.T.);
#1451=ORIENTED_EDGE('',*,*,#1109,.F.);
#1452=ORIENTED_EDGE('',*,*,#1108,.F.);
#1453=ORIENTED_EDGE('',*,*,#1110,.T.);
#1454=ORIENTED_EDGE('',*,*,#1111,.T.);
#1455=ORIENTED_EDGE('',*,*,#1112,.F.);
#1456=ORIENTED_EDGE('',*,*,#1111,.F.);
#1457=ORIENTED_EDGE('',*,*,#1113,.T.);
#1458=ORIENTED_EDGE('',*,*,#1114,.T.);
#1459=ORIENTED_EDGE('',*,*,#1115,.T.);
#1460=ORIENTED_EDGE('',*,*,#1116,.T.);
#1461=ORIENTED_EDGE('',*,*,#1107,.F.);
#1462=ORIENTED_EDGE('',*,*,#1110,.F.);
#1463=ORIENTED_EDGE('',*,*,#1104,.F.);
#1464=ORIENTED_EDGE('',*,*,#1117,.T.);
#1465=ORIENTED_EDGE('',*,*,#1118,.T.);
#1466=ORIENTED_EDGE('',*,*,#1119,.T.);
#1467=ORIENTED_EDGE('',*,*,#1120,.T.);
#1468=ORIENTED_EDGE('',*,*,#1095,.F.);
#1469=ORIENTED_EDGE('',*,*,#1101,.F.);
#1470=ORIENTED_EDGE('',*,*,#1098,.F.);
#1471=ORIENTED_EDGE('',*,*,#1121,.F.);
#1472=ORIENTED_EDGE('',*,*,#1122,.F.);
#1473=ORIENTED_EDGE('',*,*,#1123,.F.);
#1474=ORIENTED_EDGE('',*,*,#1124,.F.);
#1475=ORIENTED_EDGE('',*,*,#1109,.T.);
#1476=ORIENTED_EDGE('',*,*,#1103,.T.);
#1477=ORIENTED_EDGE('',*,*,#1097,.T.);
#1478=ORIENTED_EDGE('',*,*,#1100,.T.);
#1479=ORIENTED_EDGE('',*,*,#1106,.T.);
#1480=ORIENTED_EDGE('',*,*,#1112,.T.);
#1481=ORIENTED_EDGE('',*,*,#1121,.T.);
#1482=ORIENTED_EDGE('',*,*,#1125,.F.);
#1483=ORIENTED_EDGE('',*,*,#1126,.F.);
#1484=ORIENTED_EDGE('',*,*,#1127,.T.);
#1485=ORIENTED_EDGE('',*,*,#1124,.T.);
#1486=ORIENTED_EDGE('',*,*,#1128,.F.);
#1487=ORIENTED_EDGE('',*,*,#1129,.F.);
#1488=ORIENTED_EDGE('',*,*,#1130,.T.);
#1489=ORIENTED_EDGE('',*,*,#1116,.F.);
#1490=ORIENTED_EDGE('',*,*,#1131,.F.);
#1491=ORIENTED_EDGE('',*,*,#1132,.F.);
#1492=ORIENTED_EDGE('',*,*,#1133,.T.);
#1493=ORIENTED_EDGE('',*,*,#1118,.F.);
#1494=ORIENTED_EDGE('',*,*,#1134,.F.);
#1495=ORIENTED_EDGE('',*,*,#1135,.F.);
#1496=ORIENTED_EDGE('',*,*,#1125,.T.);
#1497=ORIENTED_EDGE('',*,*,#1123,.T.);
#1498=ORIENTED_EDGE('',*,*,#1136,.F.);
#1499=ORIENTED_EDGE('',*,*,#1137,.F.);
#1500=ORIENTED_EDGE('',*,*,#1128,.T.);
#1501=ORIENTED_EDGE('',*,*,#1122,.T.);
#1502=ORIENTED_EDGE('',*,*,#1127,.F.);
#1503=ORIENTED_EDGE('',*,*,#1138,.F.);
#1504=ORIENTED_EDGE('',*,*,#1139,.T.);
#1505=ORIENTED_EDGE('',*,*,#1120,.F.);
#1506=ORIENTED_EDGE('',*,*,#1140,.F.);
#1507=ORIENTED_EDGE('',*,*,#1141,.F.);
#1508=ORIENTED_EDGE('',*,*,#1142,.T.);
#1509=ORIENTED_EDGE('',*,*,#1114,.F.);
#1510=ORIENTED_EDGE('',*,*,#1143,.F.);
#1511=ORIENTED_EDGE('',*,*,#1144,.F.);
#1512=ORIENTED_EDGE('',*,*,#1136,.T.);
#1513=ORIENTED_EDGE('',*,*,#1115,.F.);
#1514=ORIENTED_EDGE('',*,*,#1142,.F.);
#1515=ORIENTED_EDGE('',*,*,#1145,.T.);
#1516=ORIENTED_EDGE('',*,*,#1131,.T.);
#1517=ORIENTED_EDGE('',*,*,#1119,.F.);
#1518=ORIENTED_EDGE('',*,*,#1133,.F.);
#1519=ORIENTED_EDGE('',*,*,#1146,.T.);
#1520=ORIENTED_EDGE('',*,*,#1140,.T.);
#1521=ORIENTED_EDGE('',*,*,#1145,.F.);
#1522=ORIENTED_EDGE('',*,*,#1141,.T.);
#1523=ORIENTED_EDGE('',*,*,#1146,.F.);
#1524=ORIENTED_EDGE('',*,*,#1132,.T.);
#1525=ORIENTED_EDGE('',*,*,#1113,.F.);
#1526=ORIENTED_EDGE('',*,*,#1130,.F.);
#1527=ORIENTED_EDGE('',*,*,#1147,.T.);
#1528=ORIENTED_EDGE('',*,*,#1143,.T.);
#1529=ORIENTED_EDGE('',*,*,#1147,.F.);
#1530=ORIENTED_EDGE('',*,*,#1129,.T.);
#1531=ORIENTED_EDGE('',*,*,#1137,.T.);
#1532=ORIENTED_EDGE('',*,*,#1144,.T.);
#1533=ORIENTED_EDGE('',*,*,#1117,.F.);
#1534=ORIENTED_EDGE('',*,*,#1139,.F.);
#1535=ORIENTED_EDGE('',*,*,#1148,.T.);
#1536=ORIENTED_EDGE('',*,*,#1134,.T.);
#1537=ORIENTED_EDGE('',*,*,#1148,.F.);
#1538=ORIENTED_EDGE('',*,*,#1138,.T.);
#1539=ORIENTED_EDGE('',*,*,#1126,.T.);
#1540=ORIENTED_EDGE('',*,*,#1135,.T.);
#1541=ORIENTED_EDGE('',*,*,#1149,.F.);
#1542=ORIENTED_EDGE('',*,*,#1150,.T.);
#1543=ORIENTED_EDGE('',*,*,#1151,.T.);
#1544=ORIENTED_EDGE('',*,*,#1150,.F.);
#1545=ORIENTED_EDGE('',*,*,#1152,.F.);
#1546=ORIENTED_EDGE('',*,*,#1153,.T.);
#1547=ORIENTED_EDGE('',*,*,#1154,.F.);
#1548=ORIENTED_EDGE('',*,*,#1153,.F.);
#1549=ORIENTED_EDGE('',*,*,#1155,.T.);
#1550=ORIENTED_EDGE('',*,*,#1156,.T.);
#1551=ORIENTED_EDGE('',*,*,#1157,.F.);
#1552=ORIENTED_EDGE('',*,*,#1156,.F.);
#1553=ORIENTED_EDGE('',*,*,#1158,.T.);
#1554=ORIENTED_EDGE('',*,*,#1159,.T.);
#1555=ORIENTED_EDGE('',*,*,#1160,.F.);
#1556=ORIENTED_EDGE('',*,*,#1159,.F.);
#1557=ORIENTED_EDGE('',*,*,#1161,.T.);
#1558=ORIENTED_EDGE('',*,*,#1162,.T.);
#1559=ORIENTED_EDGE('',*,*,#1163,.F.);
#1560=ORIENTED_EDGE('',*,*,#1164,.T.);
#1561=ORIENTED_EDGE('',*,*,#1165,.F.);
#1562=ORIENTED_EDGE('',*,*,#1166,.T.);
#1563=ORIENTED_EDGE('',*,*,#1167,.T.);
#1564=ORIENTED_EDGE('',*,*,#1168,.T.);
#1565=ORIENTED_EDGE('',*,*,#1155,.F.);
#1566=ORIENTED_EDGE('',*,*,#1169,.F.);
#1567=ORIENTED_EDGE('',*,*,#1170,.T.);
#1568=ORIENTED_EDGE('',*,*,#1171,.T.);
#1569=ORIENTED_EDGE('',*,*,#1172,.T.);
#1570=ORIENTED_EDGE('',*,*,#1158,.F.);
#1571=ORIENTED_EDGE('',*,*,#1173,.F.);
#1572=ORIENTED_EDGE('',*,*,#1174,.F.);
#1573=ORIENTED_EDGE('',*,*,#1175,.F.);
#1574=ORIENTED_EDGE('',*,*,#1176,.F.);
#1575=ORIENTED_EDGE('',*,*,#1157,.T.);
#1576=ORIENTED_EDGE('',*,*,#1160,.T.);
#1577=ORIENTED_EDGE('',*,*,#1173,.T.);
#1578=ORIENTED_EDGE('',*,*,#1177,.F.);
#1579=ORIENTED_EDGE('',*,*,#1171,.F.);
#1580=ORIENTED_EDGE('',*,*,#1178,.T.);
#1581=ORIENTED_EDGE('',*,*,#1179,.F.);
#1582=ORIENTED_EDGE('',*,*,#1180,.T.);
#1583=ORIENTED_EDGE('',*,*,#1161,.F.);
#1584=ORIENTED_EDGE('',*,*,#1181,.T.);
#1585=ORIENTED_EDGE('',*,*,#1182,.T.);
#1586=ORIENTED_EDGE('',*,*,#1172,.F.);
#1587=ORIENTED_EDGE('',*,*,#1177,.T.);
#1588=ORIENTED_EDGE('',*,*,#1176,.T.);
#1589=ORIENTED_EDGE('',*,*,#1183,.F.);
#1590=ORIENTED_EDGE('',*,*,#1166,.F.);
#1591=ORIENTED_EDGE('',*,*,#1151,.F.);
#1592=ORIENTED_EDGE('',*,*,#1175,.T.);
#1593=ORIENTED_EDGE('',*,*,#1184,.F.);
#1594=ORIENTED_EDGE('',*,*,#1167,.F.);
#1595=ORIENTED_EDGE('',*,*,#1183,.T.);
#1596=ORIENTED_EDGE('',*,*,#1185,.F.);
#1597=ORIENTED_EDGE('',*,*,#1186,.T.);
#1598=ORIENTED_EDGE('',*,*,#1187,.T.);
#1599=ORIENTED_EDGE('',*,*,#1168,.F.);
#1600=ORIENTED_EDGE('',*,*,#1184,.T.);
#1601=ORIENTED_EDGE('',*,*,#1174,.T.);
#1602=ORIENTED_EDGE('',*,*,#1178,.F.);
#1603=ORIENTED_EDGE('',*,*,#1170,.F.);
#1604=ORIENTED_EDGE('',*,*,#1188,.F.);
#1605=ORIENTED_EDGE('',*,*,#1189,.T.);
#1606=ORIENTED_EDGE('',*,*,#1152,.T.);
#1607=ORIENTED_EDGE('',*,*,#1190,.T.);
#1608=ORIENTED_EDGE('',*,*,#1191,.T.);
#1609=ORIENTED_EDGE('',*,*,#1188,.T.);
#1610=ORIENTED_EDGE('',*,*,#1169,.T.);
#1611=ORIENTED_EDGE('',*,*,#1182,.F.);
#1612=ORIENTED_EDGE('',*,*,#1192,.T.);
#1613=ORIENTED_EDGE('',*,*,#1193,.F.);
#1614=ORIENTED_EDGE('',*,*,#1194,.F.);
#1615=ORIENTED_EDGE('',*,*,#1187,.F.);
#1616=ORIENTED_EDGE('',*,*,#1195,.T.);
#1617=ORIENTED_EDGE('',*,*,#1196,.F.);
#1618=ORIENTED_EDGE('',*,*,#1197,.F.);
#1619=ORIENTED_EDGE('',*,*,#1198,.T.);
#1620=ORIENTED_EDGE('',*,*,#1199,.T.);
#1621=ORIENTED_EDGE('',*,*,#1179,.T.);
#1622=ORIENTED_EDGE('',*,*,#1165,.T.);
#1623=ORIENTED_EDGE('',*,*,#1200,.F.);
#1624=ORIENTED_EDGE('',*,*,#1201,.T.);
#1625=ORIENTED_EDGE('',*,*,#1185,.T.);
#1626=ORIENTED_EDGE('',*,*,#1202,.T.);
#1627=ORIENTED_EDGE('',*,*,#1163,.T.);
#1628=ORIENTED_EDGE('',*,*,#1203,.T.);
#1629=ORIENTED_EDGE('',*,*,#1198,.F.);
#1630=ORIENTED_EDGE('',*,*,#1204,.F.);
#1631=ORIENTED_EDGE('',*,*,#1193,.T.);
#1632=ORIENTED_EDGE('',*,*,#1205,.T.);
#1633=ORIENTED_EDGE('',*,*,#1149,.T.);
#1634=ORIENTED_EDGE('',*,*,#1196,.T.);
#1635=ORIENTED_EDGE('',*,*,#1206,.T.);
#1636=ORIENTED_EDGE('',*,*,#1200,.T.);
#1637=ORIENTED_EDGE('',*,*,#1207,.T.);
#1638=ORIENTED_EDGE('',*,*,#1190,.F.);
#1639=ORIENTED_EDGE('',*,*,#1208,.F.);
#1640=ORIENTED_EDGE('',*,*,#1154,.T.);
#1641=ORIENTED_EDGE('',*,*,#1197,.T.);
#1642=ORIENTED_EDGE('',*,*,#1208,.T.);
#1643=ORIENTED_EDGE('',*,*,#1194,.T.);
#1644=ORIENTED_EDGE('',*,*,#1204,.T.);
#1645=ORIENTED_EDGE('',*,*,#1206,.F.);
#1646=ORIENTED_EDGE('',*,*,#1195,.F.);
#1647=ORIENTED_EDGE('',*,*,#1186,.F.);
#1648=ORIENTED_EDGE('',*,*,#1201,.F.);
#1649=ORIENTED_EDGE('',*,*,#1180,.F.);
#1650=ORIENTED_EDGE('',*,*,#1199,.F.);
#1651=ORIENTED_EDGE('',*,*,#1203,.F.);
#1652=ORIENTED_EDGE('',*,*,#1162,.F.);
#1653=ORIENTED_EDGE('',*,*,#1189,.F.);
#1654=ORIENTED_EDGE('',*,*,#1191,.F.);
#1655=ORIENTED_EDGE('',*,*,#1207,.F.);
#1656=ORIENTED_EDGE('',*,*,#1202,.F.);
#1657=ORIENTED_EDGE('',*,*,#1205,.F.);
#1658=ORIENTED_EDGE('',*,*,#1192,.F.);
#1659=ORIENTED_EDGE('',*,*,#1181,.F.);
#1660=ORIENTED_EDGE('',*,*,#1164,.F.);
#1661=ORIENTED_EDGE('',*,*,#1209,.F.);
#1662=ORIENTED_EDGE('',*,*,#1210,.T.);
#1663=ORIENTED_EDGE('',*,*,#1211,.F.);
#1664=ORIENTED_EDGE('',*,*,#1210,.F.);
#1665=ORIENTED_EDGE('',*,*,#1212,.F.);
#1666=ORIENTED_EDGE('',*,*,#1213,.F.);
#1667=ORIENTED_EDGE('',*,*,#1214,.T.);
#1668=ORIENTED_EDGE('',*,*,#1215,.F.);
#1669=ORIENTED_EDGE('',*,*,#1214,.F.);
#1670=ORIENTED_EDGE('',*,*,#1212,.T.);
#1671=ORIENTED_EDGE('',*,*,#1213,.T.);
#1672=ORIENTED_EDGE('',*,*,#1216,.T.);
#1673=ORIENTED_EDGE('',*,*,#1209,.T.);
#1674=ORIENTED_EDGE('',*,*,#1216,.F.);
#1675=ORIENTED_EDGE('',*,*,#1215,.T.);
#1676=ORIENTED_EDGE('',*,*,#1211,.T.);
#1677=TOROIDAL_SURFACE('',#1878,6.,1.5);
#1678=TOROIDAL_SURFACE('',#1882,4.49999999999999,3.);
#1679=ADVANCED_FACE('',(#512),#1677,.T.);
#1680=ADVANCED_FACE('',(#513),#1678,.T.);
#1681=ADVANCED_FACE('',(#514),#478,.T.);
#1682=ADVANCED_FACE('',(#515),#479,.T.);
#1683=ADVANCED_FACE('',(#516,#147),#480,.T.);
#1684=ADVANCED_FACE('',(#517),#88,.F.);
#1685=ADVANCED_FACE('',(#518,#148),#89,.F.);
#1686=ADVANCED_FACE('',(#519,#149),#90,.F.);
#1687=ADVANCED_FACE('',(#520),#91,.F.);
#1688=ADVANCED_FACE('',(#521),#92,.F.);
#1689=ADVANCED_FACE('',(#522),#93,.T.);
#1690=ADVANCED_FACE('',(#523),#94,.F.);
#1691=ADVANCED_FACE('',(#524),#51,.T.);
#1692=ADVANCED_FACE('',(#525),#52,.T.);
#1693=ADVANCED_FACE('',(#526),#53,.T.);
#1694=ADVANCED_FACE('',(#527),#481,.F.);
#1695=ADVANCED_FACE('',(#528),#482,.T.);
#1696=ADVANCED_FACE('',(#529,#150),#483,.F.);
#1697=ADVANCED_FACE('',(#530,#151),#484,.T.);
#1698=ADVANCED_FACE('',(#531,#152),#95,.F.);
#1699=ADVANCED_FACE('',(#532,#153),#96,.F.);
#1700=ADVANCED_FACE('',(#533,#154),#97,.F.);
#1701=ADVANCED_FACE('',(#534),#485,.F.);
#1702=ADVANCED_FACE('',(#535),#486,.F.);
#1703=ADVANCED_FACE('',(#536),#487,.F.);
#1704=ADVANCED_FACE('',(#537),#488,.F.);
#1705=ADVANCED_FACE('',(#538,#155),#98,.T.);
#1706=ADVANCED_FACE('',(#539,#156),#99,.F.);
#1707=ADVANCED_FACE('',(#540),#100,.F.);
#1708=ADVANCED_FACE('',(#541,#157,#158,#159),#101,.F.);
#1709=ADVANCED_FACE('',(#542),#102,.F.);
#1710=ADVANCED_FACE('',(#543),#103,.F.);
#1711=ADVANCED_FACE('',(#544),#104,.F.);
#1712=ADVANCED_FACE('',(#545),#105,.F.);
#1713=ADVANCED_FACE('',(#546),#106,.T.);
#1714=ADVANCED_FACE('',(#547),#107,.T.);
#1715=ADVANCED_FACE('',(#548),#108,.T.);
#1716=ADVANCED_FACE('',(#549),#489,.F.);
#1717=ADVANCED_FACE('',(#550),#490,.F.);
#1718=ADVANCED_FACE('',(#551),#491,.T.);
#1719=ADVANCED_FACE('',(#552,#160,#161),#109,.T.);
#1720=ADVANCED_FACE('',(#553,#162,#163),#110,.F.);
#1721=ADVANCED_FACE('',(#554),#492,.F.);
#1722=ADVANCED_FACE('',(#555),#493,.F.);
#1723=ADVANCED_FACE('',(#556),#494,.T.);
#1724=ADVANCED_FACE('',(#557,#164,#165),#111,.F.);
#1725=ADVANCED_FACE('',(#558,#166,#167),#112,.T.);
#1726=ADVANCED_FACE('',(#559),#495,.T.);
#1727=ADVANCED_FACE('',(#560),#113,.F.);
#1728=ADVANCED_FACE('',(#561),#114,.F.);
#1729=ADVANCED_FACE('',(#562),#496,.F.);
#1730=ADVANCED_FACE('',(#563),#115,.T.);
#1731=ADVANCED_FACE('',(#564),#116,.T.);
#1732=ADVANCED_FACE('',(#565),#497,.F.);
#1733=ADVANCED_FACE('',(#566),#498,.F.);
#1734=ADVANCED_FACE('',(#567),#499,.F.);
#1735=ADVANCED_FACE('',(#568),#500,.F.);
#1736=ADVANCED_FACE('',(#569),#501,.F.);
#1737=ADVANCED_FACE('',(#570),#502,.F.);
#1738=ADVANCED_FACE('',(#571,#168,#169,#170),#117,.T.);
#1739=ADVANCED_FACE('',(#572,#171,#172,#173),#118,.T.);
#1740=ADVANCED_FACE('',(#573,#174,#175,#176,#177,#178,#179),#119,.F.);
#1741=ADVANCED_FACE('',(#574),#120,.F.);
#1742=ADVANCED_FACE('',(#575),#121,.F.);
#1743=ADVANCED_FACE('',(#576),#122,.F.);
#1744=ADVANCED_FACE('',(#577),#123,.F.);
#1745=ADVANCED_FACE('',(#578),#124,.T.);
#1746=ADVANCED_FACE('',(#579),#125,.T.);
#1747=ADVANCED_FACE('',(#580),#126,.T.);
#1748=ADVANCED_FACE('',(#581),#127,.T.);
#1749=ADVANCED_FACE('',(#582),#128,.T.);
#1750=ADVANCED_FACE('',(#583),#129,.T.);
#1751=ADVANCED_FACE('',(#584),#130,.T.);
#1752=ADVANCED_FACE('',(#585),#503,.F.);
#1753=ADVANCED_FACE('',(#586),#504,.F.);
#1754=ADVANCED_FACE('',(#587),#505,.F.);
#1755=ADVANCED_FACE('',(#588),#506,.F.);
#1756=ADVANCED_FACE('',(#589),#131,.F.);
#1757=ADVANCED_FACE('',(#590,#180),#132,.T.);
#1758=ADVANCED_FACE('',(#591,#181),#133,.T.);
#1759=ADVANCED_FACE('',(#592,#182,#183),#134,.F.);
#1760=ADVANCED_FACE('',(#593),#135,.F.);
#1761=ADVANCED_FACE('',(#594,#184),#136,.F.);
#1762=ADVANCED_FACE('',(#595),#137,.F.);
#1763=ADVANCED_FACE('',(#596,#185),#138,.F.);
#1764=ADVANCED_FACE('',(#597),#139,.F.);
#1765=ADVANCED_FACE('',(#598),#140,.F.);
#1766=ADVANCED_FACE('',(#599),#141,.F.);
#1767=ADVANCED_FACE('',(#600,#186),#142,.F.);
#1768=ADVANCED_FACE('',(#601,#187),#143,.F.);
#1769=ADVANCED_FACE('',(#602),#144,.T.);
#1770=ADVANCED_FACE('',(#603),#507,.T.);
#1771=ADVANCED_FACE('',(#604),#508,.T.);
#1772=ADVANCED_FACE('',(#605),#509,.T.);
#1773=ADVANCED_FACE('',(#606),#510,.T.);
#1774=ADVANCED_FACE('',(#607),#54,.T.);
#1775=ADVANCED_FACE('',(#608),#55,.T.);
#1776=ADVANCED_FACE('',(#609),#511,.T.);
#1777=ADVANCED_FACE('',(#610),#145,.T.);
#1778=ADVANCED_FACE('',(#611),#146,.T.);
#1779=CLOSED_SHELL('',(#1679,#1680,#1681,#1682,#1683,#1684,#1685,#1686,
#1687,#1688,#1689,#1690));
#1780=CLOSED_SHELL('',(#1691,#1692,#1693,#1694,#1695,#1696,#1697,#1698,
#1699,#1700));
#1781=CLOSED_SHELL('',(#1701,#1702,#1703,#1704,#1705,#1706,#1707,#1708,
#1709,#1710,#1711,#1712,#1713,#1714,#1715));
#1782=CLOSED_SHELL('',(#1716,#1717,#1718,#1719,#1720));
#1783=CLOSED_SHELL('',(#1721,#1722,#1723,#1724,#1725,#1726,#1727,#1728,
#1729,#1730,#1731));
#1784=CLOSED_SHELL('',(#1732,#1733,#1734,#1735,#1736,#1737,#1738,#1739,
#1740,#1741,#1742,#1743,#1744,#1745,#1746,#1747,#1748,#1749,#1750,#1751));
#1785=CLOSED_SHELL('',(#1752,#1753,#1754,#1755,#1756,#1757,#1758,#1759,
#1760,#1761,#1762,#1763,#1764,#1765,#1766,#1767,#1768,#1769,#1770,#1771,
#1772,#1773));
#1786=CLOSED_SHELL('',(#1774,#1775,#1776,#1777,#1778));
#1787=DERIVED_UNIT_ELEMENT(#1803,1.);
#1788=DERIVED_UNIT_ELEMENT(#3208,-3.);
#1789=DERIVED_UNIT_ELEMENT(#1803,1.);
#1790=DERIVED_UNIT_ELEMENT(#3208,-3.);
#1791=DERIVED_UNIT_ELEMENT(#1803,1.);
#1792=DERIVED_UNIT_ELEMENT(#3208,-3.);
#1793=DERIVED_UNIT_ELEMENT(#1803,1.);
#1794=DERIVED_UNIT_ELEMENT(#3208,-3.);
#1795=DERIVED_UNIT_ELEMENT(#1803,1.);
#1796=DERIVED_UNIT_ELEMENT(#3208,-3.);
#1797=DERIVED_UNIT_ELEMENT(#1803,1.);
#1798=DERIVED_UNIT_ELEMENT(#3208,-3.);
#1799=DERIVED_UNIT_ELEMENT(#1803,1.);
#1800=DERIVED_UNIT_ELEMENT(#3208,-3.);
#1801=DERIVED_UNIT_ELEMENT(#1803,1.);
#1802=DERIVED_UNIT_ELEMENT(#3208,-3.);
#1803=(
MASS_UNIT()
NAMED_UNIT(*)
SI_UNIT(.KILO.,.GRAM.)
);
#1804=DERIVED_UNIT((#1787,#1788));
#1805=DERIVED_UNIT((#1789,#1790));
#1806=DERIVED_UNIT((#1791,#1792));
#1807=DERIVED_UNIT((#1793,#1794));
#1808=DERIVED_UNIT((#1795,#1796));
#1809=DERIVED_UNIT((#1797,#1798));
#1810=DERIVED_UNIT((#1799,#1800));
#1811=DERIVED_UNIT((#1801,#1802));
#1812=MEASURE_REPRESENTATION_ITEM('density measure',
POSITIVE_RATIO_MEASURE(7850.),#1804);
#1813=MEASURE_REPRESENTATION_ITEM('density measure',
POSITIVE_RATIO_MEASURE(7850.),#1805);
#1814=MEASURE_REPRESENTATION_ITEM('density measure',
POSITIVE_RATIO_MEASURE(7850.),#1806);
#1815=MEASURE_REPRESENTATION_ITEM('density measure',
POSITIVE_RATIO_MEASURE(7850.),#1807);
#1816=MEASURE_REPRESENTATION_ITEM('density measure',
POSITIVE_RATIO_MEASURE(7850.),#1808);
#1817=MEASURE_REPRESENTATION_ITEM('density measure',
POSITIVE_RATIO_MEASURE(7850.),#1809);
#1818=MEASURE_REPRESENTATION_ITEM('density measure',
POSITIVE_RATIO_MEASURE(7850.),#1810);
#1819=MEASURE_REPRESENTATION_ITEM('density measure',
POSITIVE_RATIO_MEASURE(7850.),#1811);
#1820=PROPERTY_DEFINITION_REPRESENTATION(#1860,#1836);
#1821=PROPERTY_DEFINITION_REPRESENTATION(#1861,#1837);
#1822=PROPERTY_DEFINITION_REPRESENTATION(#1862,#1838);
#1823=PROPERTY_DEFINITION_REPRESENTATION(#1863,#1839);
#1824=PROPERTY_DEFINITION_REPRESENTATION(#1864,#1840);
#1825=PROPERTY_DEFINITION_REPRESENTATION(#1865,#1841);
#1826=PROPERTY_DEFINITION_REPRESENTATION(#1866,#1842);
#1827=PROPERTY_DEFINITION_REPRESENTATION(#1867,#1843);
#1828=PROPERTY_DEFINITION_REPRESENTATION(#1868,#1844);
#1829=PROPERTY_DEFINITION_REPRESENTATION(#1869,#1845);
#1830=PROPERTY_DEFINITION_REPRESENTATION(#1870,#1846);
#1831=PROPERTY_DEFINITION_REPRESENTATION(#1871,#1847);
#1832=PROPERTY_DEFINITION_REPRESENTATION(#1872,#1848);
#1833=PROPERTY_DEFINITION_REPRESENTATION(#1873,#1849);
#1834=PROPERTY_DEFINITION_REPRESENTATION(#1874,#1850);
#1835=PROPERTY_DEFINITION_REPRESENTATION(#1875,#1851);
#1836=REPRESENTATION('material name',(#1852),#3198);
#1837=REPRESENTATION('density',(#1812),#3198);
#1838=REPRESENTATION('material name',(#1853),#3199);
#1839=REPRESENTATION('density',(#1813),#3199);
#1840=REPRESENTATION('material name',(#1854),#3200);
#1841=REPRESENTATION('density',(#1814),#3200);
#1842=REPRESENTATION('material name',(#1855),#3201);
#1843=REPRESENTATION('density',(#1815),#3201);
#1844=REPRESENTATION('material name',(#1856),#3202);
#1845=REPRESENTATION('density',(#1816),#3202);
#1846=REPRESENTATION('material name',(#1857),#3203);
#1847=REPRESENTATION('density',(#1817),#3203);
#1848=REPRESENTATION('material name',(#1858),#3204);
#1849=REPRESENTATION('density',(#1818),#3204);
#1850=REPRESENTATION('material name',(#1859),#3205);
#1851=REPRESENTATION('density',(#1819),#3205);
#1852=DESCRIPTIVE_REPRESENTATION_ITEM('Steel','Steel');
#1853=DESCRIPTIVE_REPRESENTATION_ITEM('Steel','Steel');
#1854=DESCRIPTIVE_REPRESENTATION_ITEM('Steel','Steel');
#1855=DESCRIPTIVE_REPRESENTATION_ITEM('Steel','Steel');
#1856=DESCRIPTIVE_REPRESENTATION_ITEM('Steel','Steel');
#1857=DESCRIPTIVE_REPRESENTATION_ITEM('Steel','Steel');
#1858=DESCRIPTIVE_REPRESENTATION_ITEM('Steel','Steel');
#1859=DESCRIPTIVE_REPRESENTATION_ITEM('Steel','Steel');
#1860=PROPERTY_DEFINITION('material property','material name',#3249);
#1861=PROPERTY_DEFINITION('material property','density of part',#3249);
#1862=PROPERTY_DEFINITION('material property','material name',#3250);
#1863=PROPERTY_DEFINITION('material property','density of part',#3250);
#1864=PROPERTY_DEFINITION('material property','material name',#3251);
#1865=PROPERTY_DEFINITION('material property','density of part',#3251);
#1866=PROPERTY_DEFINITION('material property','material name',#3252);
#1867=PROPERTY_DEFINITION('material property','density of part',#3252);
#1868=PROPERTY_DEFINITION('material property','material name',#3253);
#1869=PROPERTY_DEFINITION('material property','density of part',#3253);
#1870=PROPERTY_DEFINITION('material property','material name',#3254);
#1871=PROPERTY_DEFINITION('material property','density of part',#3254);
#1872=PROPERTY_DEFINITION('material property','material name',#3255);
#1873=PROPERTY_DEFINITION('material property','density of part',#3255);
#1874=PROPERTY_DEFINITION('material property','material name',#3256);
#1875=PROPERTY_DEFINITION('material property','density of part',#3256);
#1876=AXIS2_PLACEMENT_3D('',#2618,#2075,#2076);
#1877=AXIS2_PLACEMENT_3D('',#2619,#2077,#2078);
#1878=AXIS2_PLACEMENT_3D('',#2620,#2079,#2080);
#1879=AXIS2_PLACEMENT_3D('',#2622,#2081,#2082);
#1880=AXIS2_PLACEMENT_3D('',#2624,#2083,#2084);
#1881=AXIS2_PLACEMENT_3D('',#2625,#2085,#2086);
#1882=AXIS2_PLACEMENT_3D('',#2626,#2087,#2088);
#1883=AXIS2_PLACEMENT_3D('',#2629,#2089,#2090);
#1884=AXIS2_PLACEMENT_3D('',#2630,#2091,#2092);
#1885=AXIS2_PLACEMENT_3D('',#2632,#2093,#2094);
#1886=AXIS2_PLACEMENT_3D('',#2633,#2095,#2096);
#1887=AXIS2_PLACEMENT_3D('',#2634,#2097,#2098);
#1888=AXIS2_PLACEMENT_3D('',#2636,#2099,#2100);
#1889=AXIS2_PLACEMENT_3D('',#2639,#2102,#2103);
#1890=AXIS2_PLACEMENT_3D('',#2640,#2104,#2105);
#1891=AXIS2_PLACEMENT_3D('',#2642,#2106,#2107);
#1892=AXIS2_PLACEMENT_3D('',#2644,#2109,#2110);
#1893=AXIS2_PLACEMENT_3D('',#2647,#2112,#2113);
#1894=AXIS2_PLACEMENT_3D('',#2650,#2114,#2115);
#1895=AXIS2_PLACEMENT_3D('',#2654,#2117,#2118);
#1896=AXIS2_PLACEMENT_3D('',#2656,#2120,#2121);
#1897=AXIS2_PLACEMENT_3D('',#2657,#2122,#2123);
#1898=AXIS2_PLACEMENT_3D('',#2658,#2124,#2125);
#1899=AXIS2_PLACEMENT_3D('',#2659,#2126,#2127);
#1900=AXIS2_PLACEMENT_3D('',#2660,#2128,#2129);
#1901=AXIS2_PLACEMENT_3D('',#2663,#2132,#2133);
#1902=AXIS2_PLACEMENT_3D('',#2664,#2134,#2135);
#1903=AXIS2_PLACEMENT_3D('',#2665,#2136,#2137);
#1904=AXIS2_PLACEMENT_3D('',#2666,#2138,#2139);
#1905=AXIS2_PLACEMENT_3D('',#2669,#2140,#2141);
#1906=AXIS2_PLACEMENT_3D('',#2670,#2142,#2143);
#1907=AXIS2_PLACEMENT_3D('',#2673,#2145,#2146);
#1908=AXIS2_PLACEMENT_3D('',#2674,#2147,#2148);
#1909=AXIS2_PLACEMENT_3D('',#2677,#2149,#2150);
#1910=AXIS2_PLACEMENT_3D('',#2678,#2151,#2152);
#1911=AXIS2_PLACEMENT_3D('',#2681,#2154,#2155);
#1912=AXIS2_PLACEMENT_3D('',#2682,#2156,#2157);
#1913=AXIS2_PLACEMENT_3D('',#2684,#2158,#2159);
#1914=AXIS2_PLACEMENT_3D('',#2687,#2161,#2162);
#1915=AXIS2_PLACEMENT_3D('',#2688,#2163,#2164);
#1916=AXIS2_PLACEMENT_3D('',#2766,#2166,#2167);
#1917=AXIS2_PLACEMENT_3D('',#2768,#2169,#2170);
#1918=AXIS2_PLACEMENT_3D('',#2770,#2171,#2172);
#1919=AXIS2_PLACEMENT_3D('',#2773,#2174,#2175);
#1920=AXIS2_PLACEMENT_3D('',#2774,#2176,#2177);
#1921=AXIS2_PLACEMENT_3D('',#2777,#2179,#2180);
#1922=AXIS2_PLACEMENT_3D('',#2778,#2181,#2182);
#1923=AXIS2_PLACEMENT_3D('',#2779,#2183,#2184);
#1924=AXIS2_PLACEMENT_3D('',#2780,#2185,#2186);
#1925=AXIS2_PLACEMENT_3D('',#2781,#2187,#2188);
#1926=AXIS2_PLACEMENT_3D('',#2782,#2189,#2190);
#1927=AXIS2_PLACEMENT_3D('',#2784,#2191,#2192);
#1928=AXIS2_PLACEMENT_3D('',#2787,#2194,#2195);
#1929=AXIS2_PLACEMENT_3D('',#2788,#2196,#2197);
#1930=AXIS2_PLACEMENT_3D('',#2790,#2198,#2199);
#1931=AXIS2_PLACEMENT_3D('',#2793,#2201,#2202);
#1932=AXIS2_PLACEMENT_3D('',#2794,#2203,#2204);
#1933=AXIS2_PLACEMENT_3D('',#2796,#2205,#2206);
#1934=AXIS2_PLACEMENT_3D('',#2799,#2208,#2209);
#1935=AXIS2_PLACEMENT_3D('',#2800,#2210,#2211);
#1936=AXIS2_PLACEMENT_3D('',#2802,#2212,#2213);
#1937=AXIS2_PLACEMENT_3D('',#2805,#2215,#2216);
#1938=AXIS2_PLACEMENT_3D('',#2806,#2217,#2218);
#1939=AXIS2_PLACEMENT_3D('',#2819,#2225,#2226);
#1940=AXIS2_PLACEMENT_3D('',#2832,#2233,#2234);
#1941=AXIS2_PLACEMENT_3D('',#2835,#2237,#2238);
#1942=AXIS2_PLACEMENT_3D('',#2837,#2240,#2241);
#1943=AXIS2_PLACEMENT_3D('',#2839,#2243,#2244);
#1944=AXIS2_PLACEMENT_3D('',#2842,#2247,#2248);
#1945=AXIS2_PLACEMENT_3D('',#2843,#2249,#2250);
#1946=AXIS2_PLACEMENT_3D('',#2844,#2251,#2252);
#1947=AXIS2_PLACEMENT_3D('',#2845,#2253,#2254);
#1948=AXIS2_PLACEMENT_3D('',#2846,#2255,#2256);
#1949=AXIS2_PLACEMENT_3D('',#2847,#2257,#2258);
#1950=AXIS2_PLACEMENT_3D('',#2848,#2259,#2260);
#1951=AXIS2_PLACEMENT_3D('',#2850,#2261,#2262);
#1952=AXIS2_PLACEMENT_3D('',#2853,#2264,#2265);
#1953=AXIS2_PLACEMENT_3D('',#2854,#2266,#2267);
#1954=AXIS2_PLACEMENT_3D('',#2856,#2268,#2269);
#1955=AXIS2_PLACEMENT_3D('',#2859,#2271,#2272);
#1956=AXIS2_PLACEMENT_3D('',#2860,#2273,#2274);
#1957=AXIS2_PLACEMENT_3D('',#2862,#2275,#2276);
#1958=AXIS2_PLACEMENT_3D('',#2865,#2278,#2279);
#1959=AXIS2_PLACEMENT_3D('',#2866,#2280,#2281);
#1960=AXIS2_PLACEMENT_3D('',#2867,#2282,#2283);
#1961=AXIS2_PLACEMENT_3D('',#2868,#2284,#2285);
#1962=AXIS2_PLACEMENT_3D('',#2869,#2286,#2287);
#1963=AXIS2_PLACEMENT_3D('',#2872,#2288,#2289);
#1964=AXIS2_PLACEMENT_3D('',#2876,#2291,#2292);
#1965=AXIS2_PLACEMENT_3D('',#2878,#2294,#2295);
#1966=AXIS2_PLACEMENT_3D('',#2880,#2296,#2297);
#1967=AXIS2_PLACEMENT_3D('',#2883,#2299,#2300);
#1968=AXIS2_PLACEMENT_3D('',#2884,#2301,#2302);
#1969=AXIS2_PLACEMENT_3D('',#2887,#2303,#2304);
#1970=AXIS2_PLACEMENT_3D('',#2891,#2306,#2307);
#1971=AXIS2_PLACEMENT_3D('',#2893,#2309,#2310);
#1972=AXIS2_PLACEMENT_3D('',#2896,#2311,#2312);
#1973=AXIS2_PLACEMENT_3D('',#2901,#2315,#2316);
#1974=AXIS2_PLACEMENT_3D('',#2904,#2319,#2320);
#1975=AXIS2_PLACEMENT_3D('',#2907,#2321,#2322);
#1976=AXIS2_PLACEMENT_3D('',#2913,#2326,#2327);
#1977=AXIS2_PLACEMENT_3D('',#2915,#2329,#2330);
#1978=AXIS2_PLACEMENT_3D('',#2918,#2333,#2334);
#1979=AXIS2_PLACEMENT_3D('',#2919,#2335,#2336);
#1980=AXIS2_PLACEMENT_3D('',#2920,#2337,#2338);
#1981=AXIS2_PLACEMENT_3D('',#2923,#2341,#2342);
#1982=AXIS2_PLACEMENT_3D('',#2924,#2343,#2344);
#1983=AXIS2_PLACEMENT_3D('',#2925,#2345,#2346);
#1984=AXIS2_PLACEMENT_3D('',#2926,#2347,#2348);
#1985=AXIS2_PLACEMENT_3D('',#2928,#2349,#2350);
#1986=AXIS2_PLACEMENT_3D('',#2931,#2352,#2353);
#1987=AXIS2_PLACEMENT_3D('',#2932,#2354,#2355);
#1988=AXIS2_PLACEMENT_3D('',#2934,#2356,#2357);
#1989=AXIS2_PLACEMENT_3D('',#2937,#2359,#2360);
#1990=AXIS2_PLACEMENT_3D('',#2938,#2361,#2362);
#1991=AXIS2_PLACEMENT_3D('',#2940,#2363,#2364);
#1992=AXIS2_PLACEMENT_3D('',#2943,#2366,#2367);
#1993=AXIS2_PLACEMENT_3D('',#2944,#2368,#2369);
#1994=AXIS2_PLACEMENT_3D('',#2946,#2370,#2371);
#1995=AXIS2_PLACEMENT_3D('',#2949,#2373,#2374);
#1996=AXIS2_PLACEMENT_3D('',#2950,#2375,#2376);
#1997=AXIS2_PLACEMENT_3D('',#2952,#2377,#2378);
#1998=AXIS2_PLACEMENT_3D('',#2955,#2380,#2381);
#1999=AXIS2_PLACEMENT_3D('',#2956,#2382,#2383);
#2000=AXIS2_PLACEMENT_3D('',#2958,#2384,#2385);
#2001=AXIS2_PLACEMENT_3D('',#2961,#2387,#2388);
#2002=AXIS2_PLACEMENT_3D('',#2962,#2389,#2390);
#2003=AXIS2_PLACEMENT_3D('',#2971,#2395,#2396);
#2004=AXIS2_PLACEMENT_3D('',#2980,#2401,#2402);
#2005=AXIS2_PLACEMENT_3D('',#2989,#2407,#2408);
#2006=AXIS2_PLACEMENT_3D('',#2995,#2412,#2413);
#2007=AXIS2_PLACEMENT_3D('',#3009,#2422,#2423);
#2008=AXIS2_PLACEMENT_3D('',#3013,#2426,#2427);
#2009=AXIS2_PLACEMENT_3D('',#3025,#2435,#2436);
#2010=AXIS2_PLACEMENT_3D('',#3027,#2438,#2439);
#2011=AXIS2_PLACEMENT_3D('',#3029,#2441,#2442);
#2012=AXIS2_PLACEMENT_3D('',#3030,#2443,#2444);
#2013=AXIS2_PLACEMENT_3D('',#3032,#2446,#2447);
#2014=AXIS2_PLACEMENT_3D('',#3033,#2448,#2449);
#2015=AXIS2_PLACEMENT_3D('',#3035,#2451,#2452);
#2016=AXIS2_PLACEMENT_3D('',#3036,#2453,#2454);
#2017=AXIS2_PLACEMENT_3D('',#3037,#2455,#2456);
#2018=AXIS2_PLACEMENT_3D('',#3039,#2457,#2458);
#2019=AXIS2_PLACEMENT_3D('',#3042,#2460,#2461);
#2020=AXIS2_PLACEMENT_3D('',#3043,#2462,#2463);
#2021=AXIS2_PLACEMENT_3D('',#3045,#2464,#2465);
#2022=AXIS2_PLACEMENT_3D('',#3048,#2467,#2468);
#2023=AXIS2_PLACEMENT_3D('',#3049,#2469,#2470);
#2024=AXIS2_PLACEMENT_3D('',#3051,#2471,#2472);
#2025=AXIS2_PLACEMENT_3D('',#3054,#2474,#2475);
#2026=AXIS2_PLACEMENT_3D('',#3055,#2476,#2477);
#2027=AXIS2_PLACEMENT_3D('',#3057,#2478,#2479);
#2028=AXIS2_PLACEMENT_3D('',#3060,#2481,#2482);
#2029=AXIS2_PLACEMENT_3D('',#3061,#2483,#2484);
#2030=AXIS2_PLACEMENT_3D('',#3070,#2489,#2490);
#2031=AXIS2_PLACEMENT_3D('',#3079,#2495,#2496);
#2032=AXIS2_PLACEMENT_3D('',#3088,#2501,#2502);
#2033=AXIS2_PLACEMENT_3D('',#3097,#2507,#2508);
#2034=AXIS2_PLACEMENT_3D('',#3100,#2511,#2512);
#2035=AXIS2_PLACEMENT_3D('',#3103,#2514,#2515);
#2036=AXIS2_PLACEMENT_3D('',#3105,#2516,#2517);
#2037=AXIS2_PLACEMENT_3D('',#3108,#2520,#2521);
#2038=AXIS2_PLACEMENT_3D('',#3110,#2523,#2524);
#2039=AXIS2_PLACEMENT_3D('',#3115,#2526,#2527);
#2040=AXIS2_PLACEMENT_3D('',#3119,#2530,#2531);
#2041=AXIS2_PLACEMENT_3D('',#3120,#2532,#2533);
#2042=AXIS2_PLACEMENT_3D('',#3130,#2539,#2540);
#2043=AXIS2_PLACEMENT_3D('',#3140,#2546,#2547);
#2044=AXIS2_PLACEMENT_3D('',#3146,#2551,#2552);
#2045=AXIS2_PLACEMENT_3D('',#3147,#2553,#2554);
#2046=AXIS2_PLACEMENT_3D('',#3149,#2556,#2557);
#2047=AXIS2_PLACEMENT_3D('',#3150,#2558,#2559);
#2048=AXIS2_PLACEMENT_3D('',#3151,#2560,#2561);
#2049=AXIS2_PLACEMENT_3D('',#3152,#2562,#2563);
#2050=AXIS2_PLACEMENT_3D('',#3154,#2565,#2566);
#2051=AXIS2_PLACEMENT_3D('',#3155,#2567,#2568);
#2052=AXIS2_PLACEMENT_3D('',#3156,#2569,#2570);
#2053=AXIS2_PLACEMENT_3D('',#3157,#2571,#2572);
#2054=AXIS2_PLACEMENT_3D('',#3158,#2573,#2574);
#2055=AXIS2_PLACEMENT_3D('',#3159,#2575,#2576);
#2056=AXIS2_PLACEMENT_3D('',#3160,#2577,#2578);
#2057=AXIS2_PLACEMENT_3D('',#3162,#2579,#2580);
#2058=AXIS2_PLACEMENT_3D('',#3165,#2582,#2583);
#2059=AXIS2_PLACEMENT_3D('',#3166,#2584,#2585);
#2060=AXIS2_PLACEMENT_3D('',#3169,#2586,#2587);
#2061=AXIS2_PLACEMENT_3D('',#3170,#2588,#2589);
#2062=AXIS2_PLACEMENT_3D('',#3173,#2591,#2592);
#2063=AXIS2_PLACEMENT_3D('',#3174,#2593,#2594);
#2064=AXIS2_PLACEMENT_3D('',#3176,#2596,#2597);
#2065=AXIS2_PLACEMENT_3D('',#3177,#2598,#2599);
#2066=AXIS2_PLACEMENT_3D('',#3178,#2600,#2601);
#2067=AXIS2_PLACEMENT_3D('',#3179,#2602,#2603);
#2068=AXIS2_PLACEMENT_3D('',#3180,#2604,#2605);
#2069=AXIS2_PLACEMENT_3D('',#3181,#2606,#2607);
#2070=AXIS2_PLACEMENT_3D('',#3182,#2608,#2609);
#2071=AXIS2_PLACEMENT_3D('',#3183,#2610,#2611);
#2072=AXIS2_PLACEMENT_3D('',#3184,#2612,#2613);
#2073=AXIS2_PLACEMENT_3D('',#3185,#2614,#2615);
#2074=AXIS2_PLACEMENT_3D('',#3186,#2616,#2617);
#2075=DIRECTION('axis',(0.,0.,1.));
#2076=DIRECTION('refdir',(1.,0.,0.));
#2077=DIRECTION('axis',(0.,0.,1.));
#2078=DIRECTION('refdir',(1.,0.,0.));
#2079=DIRECTION('center_axis',(-1.,0.,0.));
#2080=DIRECTION('ref_axis',(0.,0.,1.));
#2081=DIRECTION('center_axis',(-1.,0.,0.));
#2082=DIRECTION('ref_axis',(0.,0.,1.));
#2083=DIRECTION('center_axis',(0.,-1.,1.22587125635694E-16));
#2084=DIRECTION('ref_axis',(0.,-1.22587125635694E-16,-1.));
#2085=DIRECTION('center_axis',(1.,0.,0.));
#2086=DIRECTION('ref_axis',(0.,0.,1.));
#2087=DIRECTION('center_axis',(1.,0.,0.));
#2088=DIRECTION('ref_axis',(0.,0.,-1.));
#2089=DIRECTION('center_axis',(1.,0.,0.));
#2090=DIRECTION('ref_axis',(0.,0.,-1.));
#2091=DIRECTION('center_axis',(1.,0.,0.));
#2092=DIRECTION('ref_axis',(0.,0.,-1.));
#2093=DIRECTION('center_axis',(0.,-1.,-1.22587125635694E-16));
#2094=DIRECTION('ref_axis',(0.,-1.22587125635694E-16,1.));
#2095=DIRECTION('center_axis',(-1.,0.,0.));
#2096=DIRECTION('ref_axis',(0.,0.,-1.));
#2097=DIRECTION('center_axis',(-1.,0.,0.));
#2098=DIRECTION('ref_axis',(0.,0.,1.));
#2099=DIRECTION('center_axis',(-1.,0.,0.));
#2100=DIRECTION('ref_axis',(0.,0.,1.));
#2101=DIRECTION('',(1.,0.,0.));
#2102=DIRECTION('center_axis',(-1.,0.,0.));
#2103=DIRECTION('ref_axis',(0.,0.,1.));
#2104=DIRECTION('center_axis',(-1.,0.,0.));
#2105=DIRECTION('ref_axis',(0.,0.,1.));
#2106=DIRECTION('center_axis',(-1.,0.,0.));
#2107=DIRECTION('ref_axis',(0.,0.,1.));
#2108=DIRECTION('',(1.,0.,0.));
#2109=DIRECTION('center_axis',(-1.,0.,0.));
#2110=DIRECTION('ref_axis',(0.,0.,1.));
#2111=DIRECTION('',(1.,0.,0.));
#2112=DIRECTION('center_axis',(-1.,0.,0.));
#2113=DIRECTION('ref_axis',(0.,0.,1.));
#2114=DIRECTION('center_axis',(1.,0.,0.));
#2115=DIRECTION('ref_axis',(0.,0.,-1.));
#2116=DIRECTION('',(1.,0.,0.));
#2117=DIRECTION('center_axis',(1.,0.,0.));
#2118=DIRECTION('ref_axis',(0.,0.,-1.));
#2119=DIRECTION('',(-1.,0.,0.));
#2120=DIRECTION('center_axis',(-1.,0.,0.));
#2121=DIRECTION('ref_axis',(0.,0.,1.));
#2122=DIRECTION('center_axis',(-1.,0.,0.));
#2123=DIRECTION('ref_axis',(0.,0.,1.));
#2124=DIRECTION('center_axis',(1.,0.,0.));
#2125=DIRECTION('ref_axis',(0.,0.,-1.));
#2126=DIRECTION('center_axis',(1.,0.,0.));
#2127=DIRECTION('ref_axis',(0.,0.,-1.));
#2128=DIRECTION('center_axis',(0.,-1.,0.));
#2129=DIRECTION('ref_axis',(0.,0.,-1.));
#2130=DIRECTION('',(0.,0.,-1.));
#2131=DIRECTION('',(0.,0.,-1.));
#2132=DIRECTION('center_axis',(1.,0.,0.));
#2133=DIRECTION('ref_axis',(0.,0.,-1.));
#2134=DIRECTION('center_axis',(1.,0.,0.));
#2135=DIRECTION('ref_axis',(0.,0.,-1.));
#2136=DIRECTION('axis',(0.,0.,1.));
#2137=DIRECTION('refdir',(1.,0.,0.));
#2138=DIRECTION('center_axis',(1.,0.,0.));
#2139=DIRECTION('ref_axis',(0.,0.,-1.));
#2140=DIRECTION('center_axis',(1.,0.,0.));
#2141=DIRECTION('ref_axis',(0.,0.,-1.));
#2142=DIRECTION('center_axis',(1.,0.,0.));
#2143=DIRECTION('ref_axis',(0.,0.,-1.));
#2144=DIRECTION('',(-0.70710678118655,8.6595605623549E-17,-0.707106781186545));
#2145=DIRECTION('center_axis',(-1.,0.,0.));
#2146=DIRECTION('ref_axis',(0.,0.,-1.));
#2147=DIRECTION('center_axis',(1.,0.,0.));
#2148=DIRECTION('ref_axis',(0.,0.,-1.));
#2149=DIRECTION('center_axis',(1.,0.,0.));
#2150=DIRECTION('ref_axis',(0.,0.,-1.));
#2151=DIRECTION('center_axis',(1.,0.,0.));
#2152=DIRECTION('ref_axis',(0.,0.,-1.));
#2153=DIRECTION('',(-0.707106781186548,8.65956056235493E-17,-0.707106781186547));
#2154=DIRECTION('center_axis',(-1.,0.,0.));
#2155=DIRECTION('ref_axis',(0.,0.,-1.));
#2156=DIRECTION('center_axis',(-1.,0.,0.));
#2157=DIRECTION('ref_axis',(0.,0.,1.));
#2158=DIRECTION('center_axis',(-1.,0.,0.));
#2159=DIRECTION('ref_axis',(0.,0.,1.));
#2160=DIRECTION('',(0.707106781186545,8.65956056235496E-17,0.70710678118655));
#2161=DIRECTION('center_axis',(1.,0.,0.));
#2162=DIRECTION('ref_axis',(0.,0.,1.));
#2163=DIRECTION('center_axis',(0.,-1.,0.));
#2164=DIRECTION('ref_axis',(0.,0.,-1.));
#2165=DIRECTION('',(0.,-1.,0.));
#2166=DIRECTION('center_axis',(-1.,0.,0.));
#2167=DIRECTION('ref_axis',(0.,0.,1.));
#2168=DIRECTION('',(1.,0.,0.));
#2169=DIRECTION('center_axis',(1.,0.,0.));
#2170=DIRECTION('ref_axis',(0.,0.,-1.));
#2171=DIRECTION('center_axis',(1.,0.,0.));
#2172=DIRECTION('ref_axis',(0.,0.,-1.));
#2173=DIRECTION('',(1.,0.,0.));
#2174=DIRECTION('center_axis',(1.,0.,0.));
#2175=DIRECTION('ref_axis',(0.,0.,-1.));
#2176=DIRECTION('center_axis',(-1.,0.,0.));
#2177=DIRECTION('ref_axis',(0.,0.,1.));
#2178=DIRECTION('',(1.,0.,0.));
#2179=DIRECTION('center_axis',(-1.,0.,0.));
#2180=DIRECTION('ref_axis',(0.,0.,1.));
#2181=DIRECTION('center_axis',(-1.,0.,0.));
#2182=DIRECTION('ref_axis',(0.,0.,1.));
#2183=DIRECTION('center_axis',(1.,0.,0.));
#2184=DIRECTION('ref_axis',(0.,0.,-1.));
#2185=DIRECTION('center_axis',(1.,0.,0.));
#2186=DIRECTION('ref_axis',(0.,0.,-1.));
#2187=DIRECTION('axis',(0.,0.,1.));
#2188=DIRECTION('refdir',(1.,0.,0.));
#2189=DIRECTION('center_axis',(1.04083408558608E-17,-1.,-1.5392995080515E-31));
#2190=DIRECTION('ref_axis',(-1.60215539590589E-48,1.5392995080515E-31,-1.));
#2191=DIRECTION('center_axis',(1.04083408558608E-17,-1.,-1.5392995080515E-31));
#2192=DIRECTION('ref_axis',(-1.60215539590589E-48,1.5392995080515E-31,-1.));
#2193=DIRECTION('',(1.04083408558608E-17,-1.,-1.5392995080515E-31));
#2194=DIRECTION('center_axis',(1.04083408558608E-17,-1.,-1.5392995080515E-31));
#2195=DIRECTION('ref_axis',(-1.60215539590589E-48,1.5392995080515E-31,-1.));
#2196=DIRECTION('center_axis',(1.04083408558608E-17,-1.,-1.5392995080515E-31));
#2197=DIRECTION('ref_axis',(-1.60215539590589E-48,1.5392995080515E-31,-1.));
#2198=DIRECTION('center_axis',(1.04083408558608E-17,-1.,-1.5392995080515E-31));
#2199=DIRECTION('ref_axis',(-1.60215539590589E-48,1.5392995080515E-31,-1.));
#2200=DIRECTION('',(1.04083408558608E-17,-1.,-1.5392995080515E-31));
#2201=DIRECTION('center_axis',(1.04083408558608E-17,-1.,-1.5392995080515E-31));
#2202=DIRECTION('ref_axis',(-1.60215539590589E-48,1.5392995080515E-31,-1.));
#2203=DIRECTION('center_axis',(1.04083408558608E-17,-1.,-1.5392995080515E-31));
#2204=DIRECTION('ref_axis',(-1.60215539590589E-48,1.5392995080515E-31,-1.));
#2205=DIRECTION('center_axis',(1.04083408558608E-17,-1.,-1.5392995080515E-31));
#2206=DIRECTION('ref_axis',(-1.60215539590589E-48,1.5392995080515E-31,-1.));
#2207=DIRECTION('',(1.04083408558608E-17,-1.,-1.5392995080515E-31));
#2208=DIRECTION('center_axis',(1.04083408558608E-17,-1.,-1.5392995080515E-31));
#2209=DIRECTION('ref_axis',(-1.60215539590589E-48,1.5392995080515E-31,-1.));
#2210=DIRECTION('center_axis',(6.16297582203915E-33,-1.47526233740062E-31,
-1.));
#2211=DIRECTION('ref_axis',(-1.,-9.09200611656501E-64,-6.16297582203915E-33));
#2212=DIRECTION('center_axis',(-6.16297582203915E-33,1.47526233740062E-31,
1.));
#2213=DIRECTION('ref_axis',(1.,9.09200611656501E-64,6.16297582203915E-33));
#2214=DIRECTION('',(6.16297582203915E-33,-1.47526233740062E-31,-1.));
#2215=DIRECTION('center_axis',(-6.16297582203915E-33,1.47526233740062E-31,
1.));
#2216=DIRECTION('ref_axis',(1.,9.09200611656501E-64,6.16297582203915E-33));
#2217=DIRECTION('center_axis',(4.62223186652936E-33,1.47526233740062E-31,
1.));
#2218=DIRECTION('ref_axis',(1.,1.04083408558608E-17,-4.62223186652936E-33));
#2219=DIRECTION('',(-1.,-1.04083408558608E-17,6.16297582203915E-33));
#2220=DIRECTION('',(-0.707106781186549,-0.707106781186546,-7.08742219534503E-32));
#2221=DIRECTION('',(1.04083408558608E-17,-1.,-1.5392995080515E-31));
#2222=DIRECTION('',(1.,1.04083408558608E-17,-6.16297582203915E-33));
#2223=DIRECTION('',(-1.04083408558608E-17,1.,1.5383365430793E-31));
#2224=DIRECTION('',(-0.707106781186546,0.707106781186549,7.70371977754894E-32));
#2225=DIRECTION('center_axis',(4.62223186652936E-33,1.47526233740062E-31,
1.));
#2226=DIRECTION('ref_axis',(1.,1.04083408558608E-17,-4.62223186652936E-33));
#2227=DIRECTION('',(1.04083408558608E-17,-1.,-1.5392995080515E-31));
#2228=DIRECTION('',(0.707106781186549,0.707106781186546,7.08742219534503E-32));
#2229=DIRECTION('',(-1.,-1.04083408558608E-17,6.16297582203915E-33));
#2230=DIRECTION('',(0.707106781186546,-0.707106781186549,-7.70371977754894E-32));
#2231=DIRECTION('',(-1.04083408558608E-17,1.,1.5392995080515E-31));
#2232=DIRECTION('',(1.,1.04083408558608E-17,-6.16297582203915E-33));
#2233=DIRECTION('center_axis',(1.,1.04083408558608E-17,6.16297582203915E-33));
#2234=DIRECTION('ref_axis',(6.16297582203915E-33,-1.47526233740062E-31,
-1.));
#2235=DIRECTION('',(6.16297582203915E-33,-1.47526233740062E-31,-1.));
#2236=DIRECTION('',(6.16297582203915E-33,-1.47526233740062E-31,-1.));
#2237=DIRECTION('center_axis',(-1.04083408558608E-17,1.,-1.47526233740062E-31));
#2238=DIRECTION('ref_axis',(-6.16297582203915E-33,1.47526233740062E-31,
1.));
#2239=DIRECTION('',(6.16297582203915E-33,-1.47526233740062E-31,-1.));
#2240=DIRECTION('center_axis',(-1.,-1.04083408558608E-17,-6.16297582203915E-33));
#2241=DIRECTION('ref_axis',(-6.16297582203915E-33,1.47526233740062E-31,
1.));
#2242=DIRECTION('',(-6.16297582203915E-33,1.47526233740062E-31,1.));
#2243=DIRECTION('center_axis',(1.04083408558608E-17,-1.,1.47526233740062E-31));
#2244=DIRECTION('ref_axis',(6.16297582203915E-33,-1.47526233740062E-31,
-1.));
#2245=DIRECTION('',(-6.16297582203915E-33,1.47526233740062E-31,1.));
#2246=DIRECTION('',(6.16297582203915E-33,-1.47526233740062E-31,-1.));
#2247=DIRECTION('center_axis',(0.707106781186546,-0.707106781186549,1.08674682276562E-31));
#2248=DIRECTION('ref_axis',(6.16297582203915E-33,-1.47526233740062E-31,
-1.));
#2249=DIRECTION('center_axis',(-0.707106781186549,-0.707106781186546,9.99589182844569E-32));
#2250=DIRECTION('ref_axis',(6.16297582203915E-33,-1.47526233740062E-31,
-1.));
#2251=DIRECTION('center_axis',(1.04083408558608E-17,-1.,1.47526233740062E-31));
#2252=DIRECTION('ref_axis',(6.16297582203915E-33,-1.47526233740062E-31,
-1.));
#2253=DIRECTION('center_axis',(1.04083408558608E-17,-1.,1.47526233740062E-31));
#2254=DIRECTION('ref_axis',(6.16297582203915E-33,-1.47526233740062E-31,
-1.));
#2255=DIRECTION('center_axis',(1.04083408558608E-17,-1.,1.47526233740062E-31));
#2256=DIRECTION('ref_axis',(6.16297582203915E-33,-1.47526233740062E-31,
-1.));
#2257=DIRECTION('axis',(0.,0.,1.));
#2258=DIRECTION('refdir',(1.,0.,0.));
#2259=DIRECTION('center_axis',(-1.87200390594439E-31,-2.8065614114583E-31,
-1.));
#2260=DIRECTION('ref_axis',(-1.,5.25389392452275E-62,1.87200390594439E-31));
#2261=DIRECTION('center_axis',(1.87200390594439E-31,2.8065614114583E-31,
1.));
#2262=DIRECTION('ref_axis',(1.,-5.25389392452275E-62,-1.87200390594439E-31));
#2263=DIRECTION('',(-1.87200390594439E-31,-2.8065614114583E-31,-1.));
#2264=DIRECTION('center_axis',(1.87200390594439E-31,2.8065614114583E-31,
1.));
#2265=DIRECTION('ref_axis',(1.,-5.25389392452275E-62,-1.87200390594439E-31));
#2266=DIRECTION('center_axis',(-1.87200390594439E-31,-2.8065614114583E-31,
-1.));
#2267=DIRECTION('ref_axis',(-1.,-2.89120579329467E-17,1.87200390594439E-31));
#2268=DIRECTION('center_axis',(1.87200390594439E-31,2.8065614114583E-31,
1.));
#2269=DIRECTION('ref_axis',(1.,2.89120579329467E-17,-1.87200390594439E-31));
#2270=DIRECTION('',(-1.87200390594439E-31,-2.8065614114583E-31,-1.));
#2271=DIRECTION('center_axis',(1.87200390594439E-31,2.8065614114583E-31,
1.));
#2272=DIRECTION('ref_axis',(1.,2.89120579329467E-17,-1.87200390594439E-31));
#2273=DIRECTION('center_axis',(-1.87200390594439E-31,-2.8065614114583E-31,
-1.));
#2274=DIRECTION('ref_axis',(-1.,-2.81089452125871E-17,1.87200390594439E-31));
#2275=DIRECTION('center_axis',(1.87200390594439E-31,2.8065614114583E-31,
1.));
#2276=DIRECTION('ref_axis',(1.,2.81089452125871E-17,-1.87200390594439E-31));
#2277=DIRECTION('',(1.87200390594439E-31,2.8065614114583E-31,1.));
#2278=DIRECTION('center_axis',(1.87200390594439E-31,2.8065614114583E-31,
1.));
#2279=DIRECTION('ref_axis',(1.,2.81089452125871E-17,-1.87200390594439E-31));
#2280=DIRECTION('center_axis',(-1.85852239633368E-31,2.8065614114583E-31,
1.));
#2281=DIRECTION('ref_axis',(1.,2.77555756156288E-17,1.85852239633368E-31));
#2282=DIRECTION('center_axis',(-1.85852239633368E-31,2.8065614114583E-31,
1.));
#2283=DIRECTION('ref_axis',(1.,2.77555756156288E-17,1.85852239633368E-31));
#2284=DIRECTION('axis',(0.,0.,1.));
#2285=DIRECTION('refdir',(1.,0.,0.));
#2286=DIRECTION('center_axis',(-1.15555796663234E-33,0.,-1.));
#2287=DIRECTION('ref_axis',(-1.,0.,1.15555796663234E-33));
#2288=DIRECTION('center_axis',(1.15555796663234E-33,0.,1.));
#2289=DIRECTION('ref_axis',(1.,0.,-1.15555796663234E-33));
#2290=DIRECTION('',(-1.15555796663234E-33,0.,-1.));
#2291=DIRECTION('center_axis',(1.15555796663234E-33,0.,1.));
#2292=DIRECTION('ref_axis',(1.,0.,-1.15555796663234E-33));
#2293=DIRECTION('',(-1.15555796663234E-33,0.,-1.));
#2294=DIRECTION('center_axis',(-1.15555796663234E-33,0.,-1.));
#2295=DIRECTION('ref_axis',(-1.,0.,1.15555796663234E-33));
#2296=DIRECTION('center_axis',(1.15555796663234E-33,0.,1.));
#2297=DIRECTION('ref_axis',(1.,0.,-1.15555796663234E-33));
#2298=DIRECTION('',(-1.15555796663234E-33,0.,-1.));
#2299=DIRECTION('center_axis',(1.15555796663234E-33,0.,1.));
#2300=DIRECTION('ref_axis',(1.,0.,-1.15555796663234E-33));
#2301=DIRECTION('center_axis',(-1.15555796663234E-33,0.,-1.));
#2302=DIRECTION('ref_axis',(-1.,0.,1.15555796663234E-33));
#2303=DIRECTION('center_axis',(1.15555796663234E-33,0.,1.));
#2304=DIRECTION('ref_axis',(1.,0.,-1.15555796663234E-33));
#2305=DIRECTION('',(-1.15555796663234E-33,0.,-1.));
#2306=DIRECTION('center_axis',(1.15555796663234E-33,0.,1.));
#2307=DIRECTION('ref_axis',(1.,0.,-1.15555796663234E-33));
#2308=DIRECTION('',(-1.15555796663234E-33,0.,-1.));
#2309=DIRECTION('center_axis',(1.15555796663234E-33,0.,-1.));
#2310=DIRECTION('ref_axis',(-1.,0.,-1.15555796663234E-33));
#2311=DIRECTION('center_axis',(1.15555796663234E-33,0.,1.));
#2312=DIRECTION('ref_axis',(-1.,0.,1.15555796663234E-33));
#2313=DIRECTION('',(-1.,0.,-1.15555796663234E-33));
#2314=DIRECTION('',(1.,0.,1.15555796663234E-33));
#2315=DIRECTION('center_axis',(1.15555796663234E-33,0.,1.));
#2316=DIRECTION('ref_axis',(1.,0.,-1.15555796663234E-33));
#2317=DIRECTION('',(1.,0.,1.15555796663234E-33));
#2318=DIRECTION('',(-1.,0.,-1.15555796663234E-33));
#2319=DIRECTION('center_axis',(1.15555796663234E-33,0.,-1.));
#2320=DIRECTION('ref_axis',(-1.,0.,-1.15555796663234E-33));
#2321=DIRECTION('center_axis',(1.15555796663234E-33,0.,1.));
#2322=DIRECTION('ref_axis',(-1.,0.,1.15555796663234E-33));
#2323=DIRECTION('',(1.,0.,1.15555796663234E-33));
#2324=DIRECTION('',(-1.,0.,-1.15555796663234E-33));
#2325=DIRECTION('',(1.,0.,1.15555796663234E-33));
#2326=DIRECTION('center_axis',(1.15555796663234E-33,0.,1.));
#2327=DIRECTION('ref_axis',(1.,0.,-1.15555796663234E-33));
#2328=DIRECTION('',(-1.,0.,-1.15555796663234E-33));
#2329=DIRECTION('center_axis',(-1.15555796663234E-33,0.,-1.));
#2330=DIRECTION('ref_axis',(1.,1.22464679914735E-16,-1.15555796663234E-33));
#2331=DIRECTION('',(-1.15555796663234E-33,0.,-1.));
#2332=DIRECTION('',(-1.15555796663234E-33,0.,-1.));
#2333=DIRECTION('center_axis',(0.,-1.,0.));
#2334=DIRECTION('ref_axis',(-1.15555796663234E-33,0.,-1.));
#2335=DIRECTION('center_axis',(0.,1.,0.));
#2336=DIRECTION('ref_axis',(1.15555796663234E-33,0.,1.));
#2337=DIRECTION('center_axis',(-1.15555796663234E-33,0.,-1.));
#2338=DIRECTION('ref_axis',(1.,1.22464679914735E-16,-1.15555796663234E-33));
#2339=DIRECTION('',(-1.15555796663234E-33,0.,-1.));
#2340=DIRECTION('',(-1.15555796663234E-33,0.,-1.));
#2341=DIRECTION('center_axis',(0.,-1.,0.));
#2342=DIRECTION('ref_axis',(-1.15555796663234E-33,0.,-1.));
#2343=DIRECTION('center_axis',(0.,1.,0.));
#2344=DIRECTION('ref_axis',(1.15555796663234E-33,0.,1.));
#2345=DIRECTION('axis',(0.,0.,1.));
#2346=DIRECTION('refdir',(1.,0.,0.));
#2347=DIRECTION('center_axis',(1.46707713513697E-31,-1.04083408558608E-17,
-1.));
#2348=DIRECTION('ref_axis',(-1.,-1.52698388843454E-48,-1.46707713513697E-31));
#2349=DIRECTION('center_axis',(-1.46707713513697E-31,1.04083408558608E-17,
1.));
#2350=DIRECTION('ref_axis',(-1.,-1.52698388843454E-48,-1.46707713513697E-31));
#2351=DIRECTION('',(1.46707713513697E-31,-1.04083408558608E-17,-1.));
#2352=DIRECTION('center_axis',(-1.46707713513697E-31,1.04083408558608E-17,
1.));
#2353=DIRECTION('ref_axis',(-1.,-1.52698388843454E-48,-1.46707713513697E-31));
#2354=DIRECTION('center_axis',(1.46707713513697E-31,-1.04083408558608E-17,
-1.));
#2355=DIRECTION('ref_axis',(-1.,-1.52698388843454E-48,-1.46707713513697E-31));
#2356=DIRECTION('center_axis',(-1.46707713513697E-31,1.04083408558608E-17,
1.));
#2357=DIRECTION('ref_axis',(-1.,-1.52698388843454E-48,-1.46707713513697E-31));
#2358=DIRECTION('',(1.46707713513697E-31,-1.04083408558608E-17,-1.));
#2359=DIRECTION('center_axis',(-1.46707713513697E-31,1.04083408558608E-17,
1.));
#2360=DIRECTION('ref_axis',(-1.,-1.52698388843454E-48,-1.46707713513697E-31));
#2361=DIRECTION('center_axis',(1.46707713513697E-31,-1.04083408558608E-17,
-1.));
#2362=DIRECTION('ref_axis',(-1.,-1.52698388843454E-48,-1.46707713513697E-31));
#2363=DIRECTION('center_axis',(-1.46707713513697E-31,1.04083408558608E-17,
1.));
#2364=DIRECTION('ref_axis',(-1.,-1.52698388843454E-48,-1.46707713513697E-31));
#2365=DIRECTION('',(1.46707713513697E-31,-1.04083408558608E-17,-1.));
#2366=DIRECTION('center_axis',(-1.46707713513697E-31,1.04083408558608E-17,
1.));
#2367=DIRECTION('ref_axis',(-1.,-1.52698388843454E-48,-1.46707713513697E-31));
#2368=DIRECTION('center_axis',(1.46707713513697E-31,-1.04083408558608E-17,
-1.));
#2369=DIRECTION('ref_axis',(-1.,-1.52698388843454E-48,-1.46707713513697E-31));
#2370=DIRECTION('center_axis',(-1.46707713513697E-31,1.04083408558608E-17,
1.));
#2371=DIRECTION('ref_axis',(1.,1.52698388843454E-48,1.46707713513697E-31));
#2372=DIRECTION('',(1.46707713513697E-31,-1.04083408558608E-17,-1.));
#2373=DIRECTION('center_axis',(-1.46707713513697E-31,1.04083408558608E-17,
1.));
#2374=DIRECTION('ref_axis',(1.,1.52698388843454E-48,1.46707713513697E-31));
#2375=DIRECTION('center_axis',(1.46707713513697E-31,-1.04083408558608E-17,
-1.));
#2376=DIRECTION('ref_axis',(-1.,-1.52698388843454E-48,-1.46707713513697E-31));
#2377=DIRECTION('center_axis',(-1.46707713513697E-31,1.04083408558608E-17,
1.));
#2378=DIRECTION('ref_axis',(1.,1.52698388843454E-48,1.46707713513697E-31));
#2379=DIRECTION('',(1.46707713513697E-31,-1.04083408558608E-17,-1.));
#2380=DIRECTION('center_axis',(-1.46707713513697E-31,1.04083408558608E-17,
1.));
#2381=DIRECTION('ref_axis',(1.,1.52698388843454E-48,1.46707713513697E-31));
#2382=DIRECTION('center_axis',(1.46707713513697E-31,-1.04083408558608E-17,
-1.));
#2383=DIRECTION('ref_axis',(-1.,-1.52698388843454E-48,-1.46707713513697E-31));
#2384=DIRECTION('center_axis',(-1.46707713513697E-31,1.04083408558608E-17,
1.));
#2385=DIRECTION('ref_axis',(1.,1.52698388843454E-48,1.46707713513697E-31));
#2386=DIRECTION('',(1.46707713513697E-31,-1.04083408558608E-17,-1.));
#2387=DIRECTION('center_axis',(-1.46707713513697E-31,1.04083408558608E-17,
1.));
#2388=DIRECTION('ref_axis',(1.,1.52698388843454E-48,1.46707713513697E-31));
#2389=DIRECTION('center_axis',(1.46659565265088E-31,1.04083408558608E-17,
1.));
#2390=DIRECTION('ref_axis',(1.,-2.77333911991762E-32,-1.46659565265088E-31));
#2391=DIRECTION('',(1.15648231731787E-16,-1.,1.04083408558608E-17));
#2392=DIRECTION('',(1.,-2.77333911991762E-32,-1.46659565265088E-31));
#2393=DIRECTION('',(-2.92741351546859E-32,1.,-1.04083408558608E-17));
#2394=DIRECTION('',(-1.,2.77333911991762E-32,1.46659565265088E-31));
#2395=DIRECTION('center_axis',(1.46659565265088E-31,1.04083408558608E-17,
1.));
#2396=DIRECTION('ref_axis',(1.,-2.77333911991762E-32,-1.46659565265088E-31));
#2397=DIRECTION('',(-2.92741351546859E-32,1.,-1.04083408558608E-17));
#2398=DIRECTION('',(-1.,2.77333911991762E-32,1.46659565265088E-31));
#2399=DIRECTION('',(2.92741351546859E-32,-1.,1.04083408558608E-17));
#2400=DIRECTION('',(1.,-2.77333911991762E-32,-1.46659565265088E-31));
#2401=DIRECTION('center_axis',(1.46659565265088E-31,1.04083408558608E-17,
1.));
#2402=DIRECTION('ref_axis',(1.,-2.77333911991762E-32,-1.46659565265088E-31));
#2403=DIRECTION('',(-2.92741351546859E-32,1.,-6.93889390390721E-18));
#2404=DIRECTION('',(1.,-2.77333911991762E-32,-1.46659565265088E-31));
#2405=DIRECTION('',(2.92741351546859E-32,-1.,6.93889390390721E-18));
#2406=DIRECTION('',(-1.,2.77333911991762E-32,1.46659565265088E-31));
#2407=DIRECTION('center_axis',(-1.,2.77333911991762E-32,-1.46707713513697E-31));
#2408=DIRECTION('ref_axis',(-1.46707713513697E-31,1.04083408558608E-17,
1.));
#2409=DIRECTION('',(1.46707713513697E-31,-1.04083408558608E-17,-1.));
#2410=DIRECTION('',(-2.92741351546859E-32,1.,-1.04083408558608E-17));
#2411=DIRECTION('',(1.46707713513697E-31,-1.04083408558608E-17,-1.));
#2412=DIRECTION('center_axis',(2.92741351546859E-32,-1.,1.04083408558608E-17));
#2413=DIRECTION('ref_axis',(1.46707713513697E-31,-1.04083408558608E-17,
-1.));
#2414=DIRECTION('',(1.46707713513697E-31,-1.04083408558608E-17,-1.));
#2415=DIRECTION('',(-1.,2.77333911991762E-32,1.46659565265088E-31));
#2416=DIRECTION('',(1.46707713513697E-31,-1.04083408558608E-17,-1.));
#2417=DIRECTION('',(1.46707713513697E-31,-1.04083408558608E-17,-1.));
#2418=DIRECTION('',(-1.,2.77333911991762E-32,1.46659565265088E-31));
#2419=DIRECTION('',(1.46707713513697E-31,-1.04083408558608E-17,-1.));
#2420=DIRECTION('',(1.46707713513697E-31,-1.04083408558608E-17,-1.));
#2421=DIRECTION('',(-1.,2.77333911991762E-32,1.46659565265088E-31));
#2422=DIRECTION('center_axis',(1.,-2.77333911991762E-32,1.46707713513697E-31));
#2423=DIRECTION('ref_axis',(1.46707713513697E-31,-1.04083408558608E-17,
-1.));
#2424=DIRECTION('',(1.46707713513697E-31,-1.04083408558608E-17,-1.));
#2425=DIRECTION('',(2.92741351546859E-32,-1.,1.04083408558608E-17));
#2426=DIRECTION('center_axis',(-2.92741351546859E-32,1.,-1.04083408558608E-17));
#2427=DIRECTION('ref_axis',(-1.46707713513697E-31,1.04083408558608E-17,
1.));
#2428=DIRECTION('',(1.,-2.77333911991762E-32,-1.46659565265088E-31));
#2429=DIRECTION('',(1.46707713513697E-31,-1.04083408558608E-17,-1.));
#2430=DIRECTION('',(1.46707713513697E-31,-1.04083408558608E-17,-1.));
#2431=DIRECTION('',(1.,-2.77333911991762E-32,-1.46659565265088E-31));
#2432=DIRECTION('',(1.46707713513697E-31,-1.04083408558608E-17,-1.));
#2433=DIRECTION('',(1.46707713513697E-31,-1.04083408558608E-17,-1.));
#2434=DIRECTION('',(1.,-2.77333911991762E-32,-1.46659565265088E-31));
#2435=DIRECTION('center_axis',(-1.,2.77333911991762E-32,-1.46707713513697E-31));
#2436=DIRECTION('ref_axis',(-1.46707713513697E-31,1.04083408558608E-17,
1.));
#2437=DIRECTION('',(-2.92741351546859E-32,1.,-1.04083408558608E-17));
#2438=DIRECTION('center_axis',(1.,-2.77333911991762E-32,1.46707713513697E-31));
#2439=DIRECTION('ref_axis',(1.46707713513697E-31,-1.04083408558608E-17,
-1.));
#2440=DIRECTION('',(2.92741351546859E-32,-1.,1.04083408558608E-17));
#2441=DIRECTION('center_axis',(1.46659565265088E-31,1.04083408558608E-17,
1.));
#2442=DIRECTION('ref_axis',(1.,-2.77333911991762E-32,-1.46659565265088E-31));
#2443=DIRECTION('center_axis',(1.,1.15648231731787E-16,-1.22103958474151E-31));
#2444=DIRECTION('ref_axis',(-1.15648231731787E-16,1.,-1.04083408558608E-17));
#2445=DIRECTION('',(1.15648231731787E-16,-1.,1.04083408558608E-17));
#2446=DIRECTION('center_axis',(1.46659565265088E-31,1.04083408558608E-17,
1.));
#2447=DIRECTION('ref_axis',(1.,-2.77333911991762E-32,-1.46659565265088E-31));
#2448=DIRECTION('center_axis',(-1.,2.77333911991762E-32,-1.46707713513697E-31));
#2449=DIRECTION('ref_axis',(-1.46707713513697E-31,1.04083408558608E-17,
1.));
#2450=DIRECTION('',(-2.92741351546859E-32,1.,-1.04083408558608E-17));
#2451=DIRECTION('center_axis',(1.46659565265088E-31,1.04083408558608E-17,
1.));
#2452=DIRECTION('ref_axis',(1.,-2.77333911991762E-32,-1.46659565265088E-31));
#2453=DIRECTION('axis',(0.,0.,1.));
#2454=DIRECTION('refdir',(1.,0.,0.));
#2455=DIRECTION('center_axis',(-2.9274135154686E-32,-1.,1.84552236920907E-31));
#2456=DIRECTION('ref_axis',(-5.40260712672226E-63,-1.84552236920907E-31,
-1.));
#2457=DIRECTION('center_axis',(-2.9274135154686E-32,-1.,1.84552236920907E-31));
#2458=DIRECTION('ref_axis',(-5.40260712672226E-63,-1.84552236920907E-31,
-1.));
#2459=DIRECTION('',(-2.9274135154686E-32,-1.,1.84552236920907E-31));
#2460=DIRECTION('center_axis',(-2.9274135154686E-32,-1.,1.84552236920907E-31));
#2461=DIRECTION('ref_axis',(-5.40260712672226E-63,-1.84552236920907E-31,
-1.));
#2462=DIRECTION('center_axis',(-2.9274135154686E-32,-1.,1.84552236920907E-31));
#2463=DIRECTION('ref_axis',(-5.40260712672226E-63,-1.84552236920907E-31,
-1.));
#2464=DIRECTION('center_axis',(-2.9274135154686E-32,-1.,1.84552236920907E-31));
#2465=DIRECTION('ref_axis',(-5.40260712672226E-63,-1.84552236920907E-31,
-1.));
#2466=DIRECTION('',(-2.9274135154686E-32,-1.,1.84552236920907E-31));
#2467=DIRECTION('center_axis',(2.9274135154686E-32,1.,-1.84552236920907E-31));
#2468=DIRECTION('ref_axis',(5.40260712672226E-63,1.84552236920907E-31,1.));
#2469=DIRECTION('center_axis',(1.04083408558608E-17,1.72178137028218E-31,
-1.));
#2470=DIRECTION('ref_axis',(-1.,1.79208873811681E-48,-1.04083408558608E-17));
#2471=DIRECTION('center_axis',(-1.04083408558608E-17,-1.72178137028218E-31,
1.));
#2472=DIRECTION('ref_axis',(-1.,1.79208873811681E-48,-1.04083408558608E-17));
#2473=DIRECTION('',(1.04083408558608E-17,1.72178137028218E-31,-1.));
#2474=DIRECTION('center_axis',(-1.04083408558608E-17,-1.72178137028218E-31,
1.));
#2475=DIRECTION('ref_axis',(-1.,1.79208873811681E-48,-1.04083408558608E-17));
#2476=DIRECTION('center_axis',(1.04083408558608E-17,1.72178137028218E-31,
-1.));
#2477=DIRECTION('ref_axis',(-1.,1.79208873811681E-48,-1.04083408558608E-17));
#2478=DIRECTION('center_axis',(-1.04083408558608E-17,-1.72178137028218E-31,
1.));
#2479=DIRECTION('ref_axis',(1.,-1.79208873811681E-48,1.04083408558608E-17));
#2480=DIRECTION('',(1.04083408558608E-17,1.72178137028218E-31,-1.));
#2481=DIRECTION('center_axis',(-1.04083408558608E-17,-1.72178137028218E-31,
1.));
#2482=DIRECTION('ref_axis',(1.,-1.79208873811681E-48,1.04083408558608E-17));
#2483=DIRECTION('center_axis',(1.04083408558608E-17,1.72178137028218E-31,
-1.));
#2484=DIRECTION('ref_axis',(-1.,-2.77333911991761E-32,-1.04083408558608E-17));
#2485=DIRECTION('',(1.,2.77333911991761E-32,1.04083408558608E-17));
#2486=DIRECTION('',(2.9274135154686E-32,1.,-1.84552236920907E-31));
#2487=DIRECTION('',(1.,2.77333911991761E-32,1.04083408558608E-17));
#2488=DIRECTION('',(-2.9274135154686E-32,-1.,1.84552236920907E-31));
#2489=DIRECTION('center_axis',(-1.04083408558608E-17,-1.72178137028218E-31,
1.));
#2490=DIRECTION('ref_axis',(1.,2.77333911991761E-32,1.04083408558608E-17));
#2491=DIRECTION('',(2.9274135154686E-32,1.,-1.84552236920907E-31));
#2492=DIRECTION('',(1.,2.92741351546859E-32,6.93889390390721E-18));
#2493=DIRECTION('',(2.9274135154686E-32,1.,-1.84552236920907E-31));
#2494=DIRECTION('',(-1.,-2.77333911991761E-32,-1.04083408558608E-17));
#2495=DIRECTION('center_axis',(-1.04083408558608E-17,-1.72178137028218E-31,
1.));
#2496=DIRECTION('ref_axis',(1.,2.77333911991761E-32,1.04083408558608E-17));
#2497=DIRECTION('',(-2.9274135154686E-32,-1.,1.84552236920907E-31));
#2498=DIRECTION('',(-1.,-2.77333911991761E-32,-1.04083408558608E-17));
#2499=DIRECTION('',(-2.9274135154686E-32,-1.,1.84552236920907E-31));
#2500=DIRECTION('',(1.,2.92741351546859E-32,6.93889390390721E-18));
#2501=DIRECTION('center_axis',(-1.04083408558608E-17,-1.72178137028218E-31,
1.));
#2502=DIRECTION('ref_axis',(1.,2.77333911991761E-32,1.04083408558608E-17));
#2503=DIRECTION('',(-2.9274135154686E-32,-1.,1.84552236920907E-31));
#2504=DIRECTION('',(-1.,3.46944695195361E-16,-1.04083408558608E-17));
#2505=DIRECTION('',(2.9274135154686E-32,1.,-1.84552236920907E-31));
#2506=DIRECTION('',(1.,2.92741351546859E-32,6.93889390390721E-18));
#2507=DIRECTION('center_axis',(1.,2.77333911991761E-32,1.04083408558608E-17));
#2508=DIRECTION('ref_axis',(1.04083408558608E-17,1.72178137028218E-31,-1.));
#2509=DIRECTION('',(1.04083408558608E-17,1.72178137028218E-31,-1.));
#2510=DIRECTION('',(1.04083408558608E-17,1.72178137028218E-31,-1.));
#2511=DIRECTION('center_axis',(2.9274135154686E-32,1.,1.72178137028218E-31));
#2512=DIRECTION('ref_axis',(-1.04083408558608E-17,-1.72178137028218E-31,
1.));
#2513=DIRECTION('',(1.04083408558608E-17,1.72178137028218E-31,-1.));
#2514=DIRECTION('center_axis',(-2.9274135154686E-32,-1.,1.84552236920907E-31));
#2515=DIRECTION('ref_axis',(-4.85722573273504E-14,1.84552236920908E-31,
1.));
#2516=DIRECTION('center_axis',(-2.9274135154686E-32,-1.,1.84552236920907E-31));
#2517=DIRECTION('ref_axis',(5.40260712672226E-63,1.84552236920907E-31,1.));
#2518=DIRECTION('',(1.04083408558608E-17,1.72178137028218E-31,-1.));
#2519=DIRECTION('',(1.04083408558608E-17,1.72178137028218E-31,-1.));
#2520=DIRECTION('center_axis',(-1.,-2.77333911991761E-32,-1.04083408558608E-17));
#2521=DIRECTION('ref_axis',(-1.04083408558608E-17,-1.72178137028218E-31,
1.));
#2522=DIRECTION('',(1.04083408558608E-17,1.72178137028218E-31,-1.));
#2523=DIRECTION('center_axis',(-3.46944695195361E-16,-1.,1.4637067577343E-31));
#2524=DIRECTION('ref_axis',(1.,-3.46944695195361E-16,1.04083408558608E-17));
#2525=DIRECTION('',(-1.,-2.77333911991761E-32,-1.04083408558608E-17));
#2526=DIRECTION('center_axis',(3.46944695195362E-16,1.,-1.4637067577343E-31));
#2527=DIRECTION('ref_axis',(1.,-3.46944695195362E-16,3.4694469519536E-14));
#2528=DIRECTION('',(1.04083408558608E-17,1.72178137028218E-31,-1.));
#2529=DIRECTION('',(1.04083408558608E-17,1.72178137028218E-31,-1.));
#2530=DIRECTION('center_axis',(3.46944695195362E-16,1.,-1.4637067577343E-31));
#2531=DIRECTION('ref_axis',(1.,-3.46944695195362E-16,5.07825294917518E-47));
#2532=DIRECTION('center_axis',(1.,2.77333911991761E-32,1.04083408558608E-17));
#2533=DIRECTION('ref_axis',(1.04083408558608E-17,1.72178137028218E-31,-1.));
#2534=DIRECTION('',(-1.04083408558608E-17,-1.72178137028218E-31,1.));
#2535=DIRECTION('',(2.9274135154686E-32,1.,-1.84552236920907E-31));
#2536=DIRECTION('',(2.9274135154686E-32,1.,-1.84552236920907E-31));
#2537=DIRECTION('',(-1.04083408558608E-17,-1.72178137028218E-31,1.));
#2538=DIRECTION('',(-2.9274135154686E-32,-1.,1.84552236920907E-31));
#2539=DIRECTION('center_axis',(-1.,-2.77333911991761E-32,-1.04083408558608E-17));
#2540=DIRECTION('ref_axis',(-1.04083408558608E-17,-1.72178137028218E-31,
1.));
#2541=DIRECTION('',(-2.9274135154686E-32,-1.,1.84552236920907E-31));
#2542=DIRECTION('',(-1.04083408558608E-17,-1.72178137028218E-31,1.));
#2543=DIRECTION('',(2.9274135154686E-32,1.,-1.84552236920907E-31));
#2544=DIRECTION('',(-1.04083408558608E-17,-1.72178137028218E-31,1.));
#2545=DIRECTION('',(-2.9274135154686E-32,-1.,1.84552236920907E-31));
#2546=DIRECTION('center_axis',(1.04083408558608E-17,1.72178137028218E-31,
-1.));
#2547=DIRECTION('ref_axis',(-1.,-2.77333911991761E-32,-1.04083408558608E-17));
#2548=DIRECTION('',(-1.,-2.77333911991761E-32,-1.04083408558608E-17));
#2549=DIRECTION('',(2.9274135154686E-32,1.,-1.84552236920907E-31));
#2550=DIRECTION('',(-2.9274135154686E-32,-1.,1.84552236920907E-31));
#2551=DIRECTION('center_axis',(-2.9274135154686E-32,-1.,-1.72178137028218E-31));
#2552=DIRECTION('ref_axis',(1.04083408558608E-17,1.72178137028218E-31,-1.));
#2553=DIRECTION('center_axis',(2.9274135154686E-32,1.,-1.84552236920907E-31));
#2554=DIRECTION('ref_axis',(-5.40260712672226E-63,-1.84552236920907E-31,
-1.));
#2555=DIRECTION('',(1.,2.77333911991761E-32,1.04083408558608E-17));
#2556=DIRECTION('center_axis',(2.9274135154686E-32,1.,-1.84552236920907E-31));
#2557=DIRECTION('ref_axis',(-1.15648231731787E-15,-1.84552236920907E-31,
-1.));
#2558=DIRECTION('center_axis',(2.9274135154686E-32,1.,1.72178137028218E-31));
#2559=DIRECTION('ref_axis',(-1.04083408558608E-17,-1.72178137028218E-31,
1.));
#2560=DIRECTION('center_axis',(-2.9274135154686E-32,-1.,1.84552236920907E-31));
#2561=DIRECTION('ref_axis',(-4.85722573273504E-14,1.84552236920908E-31,
1.));
#2562=DIRECTION('center_axis',(-2.9274135154686E-32,-1.,1.84552236920907E-31));
#2563=DIRECTION('ref_axis',(5.40260712672226E-63,1.84552236920907E-31,1.));
#2564=DIRECTION('',(-1.,-2.77333911991761E-32,-1.04083408558608E-17));
#2565=DIRECTION('center_axis',(-1.04083408558608E-17,-1.72178137028218E-31,
1.));
#2566=DIRECTION('ref_axis',(1.,2.77333911991761E-32,1.04083408558608E-17));
#2567=DIRECTION('center_axis',(2.9274135154686E-32,1.,-1.84552236920907E-31));
#2568=DIRECTION('ref_axis',(5.40260712672226E-63,1.84552236920907E-31,1.));
#2569=DIRECTION('center_axis',(2.9274135154686E-32,1.,-1.84552236920907E-31));
#2570=DIRECTION('ref_axis',(5.40260712672226E-63,1.84552236920907E-31,1.));
#2571=DIRECTION('center_axis',(-2.9274135154686E-32,-1.,1.84552236920907E-31));
#2572=DIRECTION('ref_axis',(-5.40260712672226E-63,-1.84552236920907E-31,
-1.));
#2573=DIRECTION('center_axis',(-2.9274135154686E-32,-1.,1.84552236920907E-31));
#2574=DIRECTION('ref_axis',(-5.40260712672226E-63,-1.84552236920907E-31,
-1.));
#2575=DIRECTION('axis',(0.,0.,1.));
#2576=DIRECTION('refdir',(1.,0.,0.));
#2577=DIRECTION('center_axis',(1.72563323017096E-31,-1.,-1.35585468084861E-31));
#2578=DIRECTION('ref_axis',(-5.55111512312577E-17,1.35585468084861E-31,
-1.));
#2579=DIRECTION('center_axis',(1.72563323017096E-31,-1.,-1.35585468084861E-31));
#2580=DIRECTION('ref_axis',(-8.32667268468868E-16,-1.35585468084862E-31,
1.));
#2581=DIRECTION('',(4.73432941564552E-17,0.707106781186544,-0.707106781186551));
#2582=DIRECTION('center_axis',(-1.72563323017096E-31,1.,1.35585468084861E-31));
#2583=DIRECTION('ref_axis',(5.55111512312576E-17,-1.35585468084861E-31,
1.));
#2584=DIRECTION('center_axis',(-1.72563323017096E-31,1.,1.35585468084861E-31));
#2585=DIRECTION('ref_axis',(5.55111512312576E-17,-1.35585468084861E-31,
1.));
#2586=DIRECTION('center_axis',(-1.72563323017096E-31,1.,1.35585468084861E-31));
#2587=DIRECTION('ref_axis',(-5.55111512312576E-17,1.35585468084861E-31,
-1.));
#2588=DIRECTION('center_axis',(-1.72563323017096E-31,1.,1.35585468084861E-31));
#2589=DIRECTION('ref_axis',(-5.55111512312576E-17,1.35585468084861E-31,
-1.));
#2590=DIRECTION('',(1.25847917090643E-16,-0.707106781186549,0.707106781186546));
#2591=DIRECTION('center_axis',(1.72563323017096E-31,-1.,-1.35585468084861E-31));
#2592=DIRECTION('ref_axis',(-5.55111512312576E-17,1.35585468084861E-31,
-1.));
#2593=DIRECTION('center_axis',(1.72563323017096E-31,-1.,-1.35585468084861E-31));
#2594=DIRECTION('ref_axis',(-5.55111512312576E-17,1.35585468084861E-31,
-1.));
#2595=DIRECTION('',(-1.72563323017096E-31,1.,1.35585468084861E-31));
#2596=DIRECTION('center_axis',(1.72563323017096E-31,-1.,1.10933564796704E-31));
#2597=DIRECTION('ref_axis',(-5.55111512312576E-17,-1.10933564796704E-31,
-1.));
#2598=DIRECTION('center_axis',(-1.72563323017096E-31,1.,-1.10933564796704E-31));
#2599=DIRECTION('ref_axis',(5.55111512312576E-17,1.10933564796704E-31,1.));
#2600=DIRECTION('',(0.,0.,1.));
#2601=DIRECTION('',(1.,0.,0.));
#2602=DIRECTION('',(8.33463499130063E-17,0.732678797893417,0.680574594822241));
#2603=DIRECTION('',(-8.97272744643299E-17,0.680574594822241,-0.732678797893417));
#2604=DIRECTION('',(0.,0.818411895195876,-0.574632029912965));
#2605=DIRECTION('',(1.,0.,0.));
#2606=DIRECTION('',(-1.,-5.0576321064911E-17,1.09315800902868E-17));
#2607=DIRECTION('',(-9.42924511547042E-18,-0.0296095464520361,-0.999561541256417));
#2608=DIRECTION('',(-1.,-5.4789956645066E-17,1.50985303523006E-18));
#2609=DIRECTION('',(-7.18720363926945E-18,0.10376904846511,-0.994601419957083));
#2610=DIRECTION('',(1.,4.74396913439676E-17,-5.77686580763731E-18));
#2611=DIRECTION('',(4.73707133336243E-17,-0.999934947477157,-0.01140617437424));
#2612=DIRECTION('',(5.08778245647925E-17,-0.999561541256417,0.0296095464520362));
#2613=DIRECTION('',(1.,5.05763210664553E-17,-1.0931580091957E-17));
#2614=DIRECTION('',(5.08778245647928E-17,-0.999561541256417,0.0296095464520362));
#2615=DIRECTION('',(-9.42924511547039E-18,-0.0296095464520362,-0.999561541256417));
#2616=DIRECTION('',(-1.41587709138184E-17,0.951961340443411,-0.306218233129879));
#2617=DIRECTION('',(-1.34514913536228E-17,-0.306218233129879,-0.951961340443411));
#2618=CARTESIAN_POINT('',(0.,0.,0.));
#2619=CARTESIAN_POINT('',(0.,0.,0.));
#2620=CARTESIAN_POINT('Origin',(9.56831985755466,0.0206871143368639,0.));
#2621=CARTESIAN_POINT('',(9.56831985755466,0.020687114336863,-7.5));
#2622=CARTESIAN_POINT('Origin',(9.56831985755466,0.0206871143368639,0.));
#2623=CARTESIAN_POINT('',(11.0683198575547,0.0206871143368632,-6.));
#2624=CARTESIAN_POINT('Origin',(9.56831985755466,0.0206871143368632,-6.));
#2625=CARTESIAN_POINT('Origin',(11.0683198575547,0.0206871143368639,0.));
#2626=CARTESIAN_POINT('Origin',(-57.9316801424454,0.0206871143368639,0.));
#2627=CARTESIAN_POINT('',(-57.9316801424454,0.0206871143368648,-7.49999999999999));
#2628=CARTESIAN_POINT('',(-57.9316801424454,0.020687114336863,7.49999999999999));
#2629=CARTESIAN_POINT('Origin',(-57.9316801424454,0.0206871143368639,0.));
#2630=CARTESIAN_POINT('Origin',(-57.9316801424454,0.0206871143368639,0.));
#2631=CARTESIAN_POINT('',(-60.9316801424454,0.0206871143368633,4.49999999999999));
#2632=CARTESIAN_POINT('Origin',(-57.9316801424454,0.0206871143368633,4.49999999999999));
#2633=CARTESIAN_POINT('Origin',(-60.9316801424454,0.0206871143368639,0.));
#2634=CARTESIAN_POINT('Origin',(-60.9316801424454,0.0206871143368639,0.));
#2635=CARTESIAN_POINT('',(-11.4316801424453,0.0206871143368621,-15.));
#2636=CARTESIAN_POINT('Origin',(-11.4316801424453,0.0206871143368639,0.));
#2637=CARTESIAN_POINT('',(-6.93168014244534,0.0206871143368621,-15.));
#2638=CARTESIAN_POINT('',(-60.9316801424454,0.0206871143368621,-15.));
#2639=CARTESIAN_POINT('Origin',(-6.93168014244534,0.0206871143368639,0.));
#2640=CARTESIAN_POINT('Origin',(-60.9316801424454,0.0206871143368639,0.));
#2641=CARTESIAN_POINT('',(-6.93168014244534,0.020687114336863,-7.5));
#2642=CARTESIAN_POINT('Origin',(-6.93168014244534,0.0206871143368639,0.));
#2643=CARTESIAN_POINT('',(-60.9316801424454,0.020687114336863,-7.5));
#2644=CARTESIAN_POINT('Origin',(-60.9316801424454,0.0206871143368639,0.));
#2645=CARTESIAN_POINT('',(-11.4316801424453,0.020687114336863,-7.49999999999999));
#2646=CARTESIAN_POINT('',(-60.9316801424454,0.020687114336863,-7.49999999999999));
#2647=CARTESIAN_POINT('Origin',(-11.4316801424453,0.0206871143368639,0.));
#2648=CARTESIAN_POINT('',(-41.4316801424454,5.27068711433686,-5.35607132140713));
#2649=CARTESIAN_POINT('',(-41.4316801424454,5.27068711433686,5.35607132140713));
#2650=CARTESIAN_POINT('Origin',(-41.4316801424454,0.0206871143368639,0.));
#2651=CARTESIAN_POINT('',(-32.4316801424454,5.27068711433686,-5.35607132140713));
#2652=CARTESIAN_POINT('',(-60.9316801424454,5.27068711433686,-5.35607132140713));
#2653=CARTESIAN_POINT('',(-32.4316801424454,5.27068711433686,5.35607132140713));
#2654=CARTESIAN_POINT('Origin',(-32.4316801424454,0.0206871143368639,0.));
#2655=CARTESIAN_POINT('',(-60.9316801424454,5.27068711433686,5.35607132140713));
#2656=CARTESIAN_POINT('Origin',(11.0683198575547,0.0206871143368639,0.));
#2657=CARTESIAN_POINT('Origin',(-6.93168014244535,7.52068711433686,0.));
#2658=CARTESIAN_POINT('Origin',(-11.4316801424453,15.0206871143369,0.));
#2659=CARTESIAN_POINT('Origin',(-60.9316801424454,7.52068711433686,0.));
#2660=CARTESIAN_POINT('Origin',(-41.4316801424454,5.27068711433686,0.));
#2661=CARTESIAN_POINT('',(-32.4316801424454,5.27068711433686,0.));
#2662=CARTESIAN_POINT('',(-41.4316801424454,5.27068711433686,5.84572916228895));
#2663=CARTESIAN_POINT('Origin',(-41.4316801424454,0.0206871143368639,0.));
#2664=CARTESIAN_POINT('Origin',(-32.4316801424454,0.0206871143368639,0.));
#2665=CARTESIAN_POINT('',(0.,0.,0.));
#2666=CARTESIAN_POINT('Origin',(-26.3399803187666,0.0567527576880167,-1.75047265224548E-6));
#2667=CARTESIAN_POINT('',(-24.8399803187666,0.0567527576880185,-15.0000017504727));
#2668=CARTESIAN_POINT('',(-24.8399803187666,0.0567527576880148,14.9999982495274));
#2669=CARTESIAN_POINT('Origin',(-24.8399803187666,0.0567527576880167,-1.75047265224548E-6));
#2670=CARTESIAN_POINT('Origin',(-24.8399803187666,0.0567527576880167,-1.75047265224548E-6));
#2671=CARTESIAN_POINT('',(-26.3399803187666,0.056752757688015,13.4999982495273));
#2672=CARTESIAN_POINT('',(-26.3399803187666,0.056752757688015,13.4999982495273));
#2673=CARTESIAN_POINT('Origin',(-26.3399803187666,0.0567527576880167,-1.75047265224548E-6));
#2674=CARTESIAN_POINT('Origin',(-11.3399803187666,0.0567527576880167,-1.75047265224548E-6));
#2675=CARTESIAN_POINT('',(-9.83998031876658,0.0567527576880196,-24.0000017504727));
#2676=CARTESIAN_POINT('',(-9.83998031876658,0.0567527576880137,23.9999982495274));
#2677=CARTESIAN_POINT('Origin',(-9.83998031876658,0.0567527576880167,-1.75047265224548E-6));
#2678=CARTESIAN_POINT('Origin',(-9.83998031876658,0.0567527576880167,-1.75047265224548E-6));
#2679=CARTESIAN_POINT('',(-11.3399803187666,0.0567527576880139,22.4999982495273));
#2680=CARTESIAN_POINT('',(-11.3399803187666,0.0567527576880139,22.4999982495273));
#2681=CARTESIAN_POINT('Origin',(-11.3399803187666,0.0567527576880167,-1.75047265224548E-6));
#2682=CARTESIAN_POINT('Origin',(2.16001968123339,0.0567527576880167,-1.75047265224548E-6));
#2683=CARTESIAN_POINT('',(2.16001968123339,0.0567527576880137,-24.0000017504727));
#2684=CARTESIAN_POINT('Origin',(2.16001968123339,0.0567527576880167,-1.75047265224548E-6));
#2685=CARTESIAN_POINT('',(3.6600196812334,0.0567527576880139,-22.5000017504726));
#2686=CARTESIAN_POINT('',(2.16001968123339,0.0567527576880137,-24.0000017504727));
#2687=CARTESIAN_POINT('Origin',(3.6600196812334,0.0567527576880167,-1.75047265224548E-6));
#2688=CARTESIAN_POINT('Origin',(-18.8399803187666,18.056752757688,-1.75047264877604E-6));
#2689=CARTESIAN_POINT('',(-18.8399803187666,14.3658407789422,-4.50000175047265));
#2690=CARTESIAN_POINT('',(-18.8399803187666,14.3658407789422,4.49999824952735));
#2691=CARTESIAN_POINT('Ctrl Pts',(-18.8399803187666,14.3658407789422,-4.50000175047265));
#2692=CARTESIAN_POINT('Ctrl Pts',(-19.4088961997505,14.3658407789422,-4.50000175047265));
#2693=CARTESIAN_POINT('Ctrl Pts',(-20.013141546909,14.4033218435503,-4.38558312462148));
#2694=CARTESIAN_POINT('Ctrl Pts',(-21.1206936253408,14.5360270992361,-3.92530183970913));
#2695=CARTESIAN_POINT('Ctrl Pts',(-21.6243333805236,14.6290540336233,-3.57960971939459));
#2696=CARTESIAN_POINT('Ctrl Pts',(-22.4194698323699,14.8016561969128,-2.78447326754827));
#2697=CARTESIAN_POINT('Ctrl Pts',(-22.7652536793161,14.8928206825392,-2.28078537898198));
#2698=CARTESIAN_POINT('Ctrl Pts',(-23.2256026885326,15.0212047585055,-1.17305832669546));
#2699=CARTESIAN_POINT('Ctrl Pts',(-23.3399803187666,15.056752757688,-0.568748148410651));
#2700=CARTESIAN_POINT('Ctrl Pts',(-23.3399803187666,15.056752757688,0.568744647465355));
#2701=CARTESIAN_POINT('Ctrl Pts',(-23.2256026885326,15.0212047585055,1.17305482575017));
#2702=CARTESIAN_POINT('Ctrl Pts',(-22.7652536793161,14.8928206825392,2.28078187803669));
#2703=CARTESIAN_POINT('Ctrl Pts',(-22.4194698323699,14.8016561969128,2.78446976660297));
#2704=CARTESIAN_POINT('Ctrl Pts',(-21.6243333805236,14.6290540336233,3.57960621844929));
#2705=CARTESIAN_POINT('Ctrl Pts',(-21.1206936253408,14.5360270992361,3.92529833876383));
#2706=CARTESIAN_POINT('Ctrl Pts',(-20.013141546909,14.4033218435503,4.38557962367618));
#2707=CARTESIAN_POINT('Ctrl Pts',(-19.4088961997505,14.3658407789422,4.49999824952735));
#2708=CARTESIAN_POINT('Ctrl Pts',(-18.8399803187666,14.3658407789422,4.49999824952735));
#2709=CARTESIAN_POINT('',(-18.8399803187666,6.05675275768802,4.49999824952735));
#2710=CARTESIAN_POINT('',(-18.8399803187666,18.056752757688,4.49999824952735));
#2711=CARTESIAN_POINT('',(-18.8399803187666,6.05675275768802,-4.50000175047266));
#2712=CARTESIAN_POINT('Ctrl Pts',(-18.8399803187666,6.05675275768802,4.49999824952735));
#2713=CARTESIAN_POINT('Ctrl Pts',(-19.4247798659256,6.05675275768802,4.49999824952735));
#2714=CARTESIAN_POINT('Ctrl Pts',(-20.0327174049161,6.15125943860946,4.37996991421688));
#2715=CARTESIAN_POINT('Ctrl Pts',(-21.1340415543933,6.45855603358751,3.91714882470871));
#2716=CARTESIAN_POINT('Ctrl Pts',(-21.6294259483511,6.66438066194848,3.57451365062178));
#2717=CARTESIAN_POINT('Ctrl Pts',(-22.4119630421001,7.03101594719294,2.79197655687281));
#2718=CARTESIAN_POINT('Ctrl Pts',(-22.7563617548165,7.21926420444051,2.29589436091356));
#2719=CARTESIAN_POINT('Ctrl Pts',(-23.220735898688,7.48336337711206,1.19086529875321));
#2720=CARTESIAN_POINT('Ctrl Pts',(-23.3399803187666,7.55675275768802,0.581024606426215));
#2721=CARTESIAN_POINT('Ctrl Pts',(-23.3399803187666,7.55675275768802,-0.581028107371513));
#2722=CARTESIAN_POINT('Ctrl Pts',(-23.220735898688,7.48336337711206,-1.19086879969851));
#2723=CARTESIAN_POINT('Ctrl Pts',(-22.7563617548165,7.21926420444051,-2.29589786185886));
#2724=CARTESIAN_POINT('Ctrl Pts',(-22.4119630421001,7.03101594719294,-2.79198005781811));
#2725=CARTESIAN_POINT('Ctrl Pts',(-21.6294259483511,6.66438066194849,-3.57451715156708));
#2726=CARTESIAN_POINT('Ctrl Pts',(-21.1340415543933,6.45855603358751,-3.91715232565401));
#2727=CARTESIAN_POINT('Ctrl Pts',(-20.0327174049161,6.15125943860947,-4.37997341516218));
#2728=CARTESIAN_POINT('Ctrl Pts',(-19.4247798659256,6.05675275768802,-4.50000175047265));
#2729=CARTESIAN_POINT('Ctrl Pts',(-18.8399803187666,6.05675275768802,-4.50000175047265));
#2730=CARTESIAN_POINT('Ctrl Pts',(-18.8399803187666,6.05675275768802,-4.50000175047265));
#2731=CARTESIAN_POINT('Ctrl Pts',(-18.2551807716076,6.05675275768802,-4.50000175047265));
#2732=CARTESIAN_POINT('Ctrl Pts',(-17.6472432326171,6.15125943860946,-4.37997341516218));
#2733=CARTESIAN_POINT('Ctrl Pts',(-16.5459190831399,6.45855603358751,-3.91715232565401));
#2734=CARTESIAN_POINT('Ctrl Pts',(-16.0505346891821,6.66438066194849,-3.57451715156707));
#2735=CARTESIAN_POINT('Ctrl Pts',(-15.2679975954331,7.03101594719294,-2.79198005781811));
#2736=CARTESIAN_POINT('Ctrl Pts',(-14.9235988827167,7.21926420444051,-2.29589786185886));
#2737=CARTESIAN_POINT('Ctrl Pts',(-14.4592247388452,7.48336337711206,-1.1908687996985));
#2738=CARTESIAN_POINT('Ctrl Pts',(-14.3399803187666,7.55675275768802,-0.581028107371512));
#2739=CARTESIAN_POINT('Ctrl Pts',(-14.3399803187666,7.55675275768802,0.581024606426216));
#2740=CARTESIAN_POINT('Ctrl Pts',(-14.4592247388452,7.48336337711206,1.19086529875321));
#2741=CARTESIAN_POINT('Ctrl Pts',(-14.9235988827167,7.21926420444051,2.29589436091356));
#2742=CARTESIAN_POINT('Ctrl Pts',(-15.2679975954331,7.03101594719294,2.79197655687282));
#2743=CARTESIAN_POINT('Ctrl Pts',(-16.0505346891821,6.66438066194848,3.57451365062178));
#2744=CARTESIAN_POINT('Ctrl Pts',(-16.5459190831399,6.45855603358751,3.91714882470872));
#2745=CARTESIAN_POINT('Ctrl Pts',(-17.6472432326171,6.15125943860946,4.37996991421688));
#2746=CARTESIAN_POINT('Ctrl Pts',(-18.2551807716076,6.05675275768802,4.49999824952735));
#2747=CARTESIAN_POINT('Ctrl Pts',(-18.8399803187666,6.05675275768802,4.49999824952735));
#2748=CARTESIAN_POINT('Ctrl Pts',(-18.8399803187666,14.3658407789422,4.49999824952735));
#2749=CARTESIAN_POINT('Ctrl Pts',(-18.2710644377827,14.3658407789422,4.49999824952735));
#2750=CARTESIAN_POINT('Ctrl Pts',(-17.6668190906242,14.4033218435503,4.38557962367618));
#2751=CARTESIAN_POINT('Ctrl Pts',(-16.5592670121924,14.5360270992361,3.92529833876383));
#2752=CARTESIAN_POINT('Ctrl Pts',(-16.0556272570096,14.6290540336233,3.57960621844929));
#2753=CARTESIAN_POINT('Ctrl Pts',(-15.2604908051633,14.8016561969128,2.78446976660297));
#2754=CARTESIAN_POINT('Ctrl Pts',(-14.9147069582171,14.8928206825392,2.28078187803668));
#2755=CARTESIAN_POINT('Ctrl Pts',(-14.4543579490006,15.0212047585055,1.17305482575016));
#2756=CARTESIAN_POINT('Ctrl Pts',(-14.3399803187666,15.056752757688,0.568744647465353));
#2757=CARTESIAN_POINT('Ctrl Pts',(-14.3399803187666,15.056752757688,-0.568748148410654));
#2758=CARTESIAN_POINT('Ctrl Pts',(-14.4543579490006,15.0212047585055,-1.17305832669547));
#2759=CARTESIAN_POINT('Ctrl Pts',(-14.9147069582171,14.8928206825392,-2.28078537898199));
#2760=CARTESIAN_POINT('Ctrl Pts',(-15.2604908051633,14.8016561969128,-2.78447326754827));
#2761=CARTESIAN_POINT('Ctrl Pts',(-16.0556272570096,14.6290540336233,-3.57960971939459));
#2762=CARTESIAN_POINT('Ctrl Pts',(-16.5592670121924,14.5360270992361,-3.92530183970913));
#2763=CARTESIAN_POINT('Ctrl Pts',(-17.6668190906242,14.4033218435503,-4.38558312462147));
#2764=CARTESIAN_POINT('Ctrl Pts',(-18.2710644377827,14.3658407789422,-4.50000175047265));
#2765=CARTESIAN_POINT('Ctrl Pts',(-18.8399803187666,14.3658407789422,-4.50000175047265));
#2766=CARTESIAN_POINT('Origin',(-26.3399803187666,0.0567527576880167,-1.75047265224548E-6));
#2767=CARTESIAN_POINT('',(-26.3399803187666,0.0567527576880137,-24.0000017504727));
#2768=CARTESIAN_POINT('Origin',(-27.8399803187666,0.0567527576880167,-1.75047265224548E-6));
#2769=CARTESIAN_POINT('',(-26.3399803187666,0.0567527576880158,7.49999824952735));
#2770=CARTESIAN_POINT('Origin',(-26.3399803187666,0.0567527576880167,-1.75047265224548E-6));
#2771=CARTESIAN_POINT('',(3.6600196812334,0.0567527576880158,7.49999824952735));
#2772=CARTESIAN_POINT('',(-27.8399803187666,0.0567527576880158,7.49999824952735));
#2773=CARTESIAN_POINT('Origin',(3.6600196812334,0.0567527576880167,-1.75047265224548E-6));
#2774=CARTESIAN_POINT('Origin',(-26.3399803187666,0.0567527576880167,-1.75047265224548E-6));
#2775=CARTESIAN_POINT('',(-11.3399803187666,0.0567527576880148,-15.0000017504727));
#2776=CARTESIAN_POINT('',(-26.3399803187666,0.0567527576880148,-15.0000017504727));
#2777=CARTESIAN_POINT('Origin',(-11.3399803187666,0.0567527576880167,-1.75047265224548E-6));
#2778=CARTESIAN_POINT('Origin',(3.6600196812334,0.0567527576880167,-1.75047265224548E-6));
#2779=CARTESIAN_POINT('Origin',(-11.3399803187666,24.056752757688,-1.75047264877604E-6));
#2780=CARTESIAN_POINT('Origin',(-26.3399803187666,15.056752757688,-1.75047265571493E-6));
#2781=CARTESIAN_POINT('',(0.,0.,0.));
#2782=CARTESIAN_POINT('Origin',(22.5,30.0905269290172,6.));
#2783=CARTESIAN_POINT('',(22.5,30.0905269290172,10.5));
#2784=CARTESIAN_POINT('Origin',(22.5,30.0905269290172,6.));
#2785=CARTESIAN_POINT('',(22.5,-14.9094730709829,10.5));
#2786=CARTESIAN_POINT('',(22.5,30.0905269290172,10.5));
#2787=CARTESIAN_POINT('Origin',(22.5,-14.9094730709829,6.));
#2788=CARTESIAN_POINT('Origin',(41.25,22.5905269290171,6.));
#2789=CARTESIAN_POINT('',(41.25,22.5905269290171,9.75000000000001));
#2790=CARTESIAN_POINT('Origin',(41.25,22.5905269290171,6.));
#2791=CARTESIAN_POINT('',(41.25,-14.9094730709829,9.75000000000001));
#2792=CARTESIAN_POINT('',(41.25,22.5905269290171,9.75000000000001));
#2793=CARTESIAN_POINT('Origin',(41.25,-14.9094730709829,6.));
#2794=CARTESIAN_POINT('Origin',(3.74999999999999,22.5905269290171,6.));
#2795=CARTESIAN_POINT('',(3.74999999999999,22.5905269290171,9.75));
#2796=CARTESIAN_POINT('Origin',(3.74999999999999,22.5905269290171,6.));
#2797=CARTESIAN_POINT('',(3.74999999999999,-14.9094730709828,9.75));
#2798=CARTESIAN_POINT('',(3.74999999999999,22.5905269290171,9.75));
#2799=CARTESIAN_POINT('Origin',(3.74999999999992,-14.9094730709828,6.));
#2800=CARTESIAN_POINT('Origin',(22.5,52.5905269290171,15.));
#2801=CARTESIAN_POINT('',(30.,52.5905269290171,15.));
#2802=CARTESIAN_POINT('Origin',(22.5,52.5905269290171,15.));
#2803=CARTESIAN_POINT('',(30.,52.5905269290171,-3.));
#2804=CARTESIAN_POINT('',(30.,52.5905269290171,15.));
#2805=CARTESIAN_POINT('Origin',(22.5,52.5905269290171,-3.));
#2806=CARTESIAN_POINT('Origin',(-11.2500000000001,-14.9094730709829,15.));
#2807=CARTESIAN_POINT('',(44.25,75.0905269290171,15.));
#2808=CARTESIAN_POINT('',(0.750000000000084,75.0905269290172,15.));
#2809=CARTESIAN_POINT('',(56.25,75.0905269290171,15.));
#2810=CARTESIAN_POINT('',(-11.25,63.0905269290172,15.));
#2811=CARTESIAN_POINT('',(-50.2500000000001,24.0905269290173,15.));
#2812=CARTESIAN_POINT('',(-11.2500000000001,-14.9094730709829,15.));
#2813=CARTESIAN_POINT('',(-11.2500000000001,75.0905269290171,15.));
#2814=CARTESIAN_POINT('',(56.25,-14.9094730709829,15.));
#2815=CARTESIAN_POINT('',(-11.2500000000001,-14.9094730709829,15.));
#2816=CARTESIAN_POINT('',(56.25,63.0905269290171,15.));
#2817=CARTESIAN_POINT('',(56.25,-14.9094730709829,15.));
#2818=CARTESIAN_POINT('',(61.5000000000001,57.840526929017,15.));
#2819=CARTESIAN_POINT('Origin',(-11.2500000000001,-14.9094730709829,-3.));
#2820=CARTESIAN_POINT('',(-11.25,63.0905269290171,-3.));
#2821=CARTESIAN_POINT('',(-11.2500000000001,-14.9094730709829,-3.));
#2822=CARTESIAN_POINT('',(-11.2500000000001,75.0905269290171,-3.));
#2823=CARTESIAN_POINT('',(0.75000000000007,75.0905269290171,-3.));
#2824=CARTESIAN_POINT('',(-11.25,63.0905269290171,-3.));
#2825=CARTESIAN_POINT('',(44.25,75.0905269290171,-3.));
#2826=CARTESIAN_POINT('',(56.25,75.0905269290171,-3.));
#2827=CARTESIAN_POINT('',(56.25,63.0905269290171,-3.));
#2828=CARTESIAN_POINT('',(44.25,75.0905269290171,-3.));
#2829=CARTESIAN_POINT('',(56.25,-14.9094730709829,-3.));
#2830=CARTESIAN_POINT('',(56.25,52.5905269290171,-3.));
#2831=CARTESIAN_POINT('',(-11.2500000000001,-14.9094730709829,-3.));
#2832=CARTESIAN_POINT('Origin',(-11.2500000000001,75.0905269290171,15.));
#2833=CARTESIAN_POINT('',(-11.25,63.0905269290171,15.));
#2834=CARTESIAN_POINT('',(-11.2500000000001,-14.9094730709829,15.));
#2835=CARTESIAN_POINT('Origin',(-11.2500000000001,-14.9094730709829,15.));
#2836=CARTESIAN_POINT('',(56.25,-14.9094730709829,15.));
#2837=CARTESIAN_POINT('Origin',(56.25,52.5905269290171,15.));
#2838=CARTESIAN_POINT('',(56.25,63.0905269290171,15.));
#2839=CARTESIAN_POINT('Origin',(56.25,75.0905269290171,15.));
#2840=CARTESIAN_POINT('',(0.750000000000056,75.0905269290171,15.));
#2841=CARTESIAN_POINT('',(44.25,75.0905269290171,15.));
#2842=CARTESIAN_POINT('Origin',(-11.25,63.0905269290171,15.));
#2843=CARTESIAN_POINT('Origin',(44.25,75.0905269290171,15.));
#2844=CARTESIAN_POINT('Origin',(3.74999999999999,22.5905269290171,6.));
#2845=CARTESIAN_POINT('Origin',(41.25,22.5905269290171,6.));
#2846=CARTESIAN_POINT('Origin',(22.5,30.0905269290172,6.));
#2847=CARTESIAN_POINT('',(0.,0.,0.));
#2848=CARTESIAN_POINT('Origin',(-6.93889390390723E-15,22.6429327686607,
12.5));
#2849=CARTESIAN_POINT('',(4.50000000000001,22.6429327686607,12.5));
#2850=CARTESIAN_POINT('Origin',(-6.93889390390723E-15,22.6429327686607,
12.5));
#2851=CARTESIAN_POINT('',(4.50000000000001,22.6429327686607,-2.5));
#2852=CARTESIAN_POINT('',(4.50000000000001,22.6429327686607,12.5));
#2853=CARTESIAN_POINT('Origin',(-6.93889390390723E-15,22.6429327686607,
-2.5));
#2854=CARTESIAN_POINT('Origin',(0.,0.142932768660666,12.5));
#2855=CARTESIAN_POINT('',(7.50000000000002,0.142932768660665,12.5));
#2856=CARTESIAN_POINT('Origin',(0.,0.142932768660666,12.5));
#2857=CARTESIAN_POINT('',(7.50000000000002,0.142932768660665,-2.5));
#2858=CARTESIAN_POINT('',(7.50000000000002,0.142932768660665,12.5));
#2859=CARTESIAN_POINT('Origin',(0.,0.142932768660666,-2.5));
#2860=CARTESIAN_POINT('Origin',(0.,0.142932768660666,12.5));
#2861=CARTESIAN_POINT('',(33.7500000000001,0.142932768660662,-2.5));
#2862=CARTESIAN_POINT('Origin',(0.,0.142932768660666,-2.5));
#2863=CARTESIAN_POINT('',(33.7500000000001,0.142932768660662,12.5));
#2864=CARTESIAN_POINT('',(33.7500000000001,0.142932768660662,12.5));
#2865=CARTESIAN_POINT('Origin',(0.,0.142932768660666,12.5));
#2866=CARTESIAN_POINT('Origin',(0.,0.142932768660666,12.5));
#2867=CARTESIAN_POINT('Origin',(0.,0.142932768660666,-2.5));
#2868=CARTESIAN_POINT('',(0.,0.,0.));
#2869=CARTESIAN_POINT('Origin',(3.22849876867702,3.46944695195361E-14,10.));
#2870=CARTESIAN_POINT('',(3.22849876867702,6.00000000000004,10.));
#2871=CARTESIAN_POINT('',(3.22849876867701,-5.99999999999996,10.));
#2872=CARTESIAN_POINT('Origin',(3.22849876867702,3.46944695195361E-14,10.));
#2873=CARTESIAN_POINT('',(3.22849876867702,-5.99999999999996,-2.));
#2874=CARTESIAN_POINT('',(3.22849876867701,-5.99999999999996,10.));
#2875=CARTESIAN_POINT('',(3.22849876867702,6.00000000000004,-2.));
#2876=CARTESIAN_POINT('Origin',(3.22849876867702,3.46944695195361E-14,-2.));
#2877=CARTESIAN_POINT('',(3.22849876867702,6.00000000000004,10.));
#2878=CARTESIAN_POINT('Origin',(-8.77150123132294,0.,10.));
#2879=CARTESIAN_POINT('',(-4.27150123132294,-5.51091059616309E-16,10.));
#2880=CARTESIAN_POINT('Origin',(-8.77150123132294,0.,10.));
#2881=CARTESIAN_POINT('',(-4.27150123132294,-5.51091059616309E-16,-2.));
#2882=CARTESIAN_POINT('',(-4.27150123132294,-5.51091059616309E-16,10.));
#2883=CARTESIAN_POINT('Origin',(-8.77150123132295,0.,-2.));
#2884=CARTESIAN_POINT('Origin',(-8.77150123132294,0.,10.));
#2885=CARTESIAN_POINT('',(-8.77150123132294,11.2500000000001,10.));
#2886=CARTESIAN_POINT('',(-8.77150123132298,-11.25,10.));
#2887=CARTESIAN_POINT('Origin',(-8.77150123132294,0.,10.));
#2888=CARTESIAN_POINT('',(-8.77150123132295,11.2500000000001,-2.));
#2889=CARTESIAN_POINT('',(-8.77150123132294,11.2500000000001,10.));
#2890=CARTESIAN_POINT('',(-8.771501231323,-11.25,-2.));
#2891=CARTESIAN_POINT('Origin',(-8.77150123132295,0.,-2.));
#2892=CARTESIAN_POINT('',(-8.77150123132298,-11.25,10.));
#2893=CARTESIAN_POINT('Origin',(48.228498768677,4.16333634234434E-14,10.));
#2894=CARTESIAN_POINT('',(48.228498768677,-11.25,10.));
#2895=CARTESIAN_POINT('',(48.228498768677,11.25,10.));
#2896=CARTESIAN_POINT('Origin',(48.228498768677,4.16333634234434E-14,10.));
#2897=CARTESIAN_POINT('',(-8.77150123132294,11.2500000000001,10.));
#2898=CARTESIAN_POINT('',(48.228498768677,-11.25,10.));
#2899=CARTESIAN_POINT('',(48.228498768677,-5.99999999999996,10.));
#2900=CARTESIAN_POINT('',(48.228498768677,6.00000000000004,10.));
#2901=CARTESIAN_POINT('Origin',(48.228498768677,4.16333634234434E-14,10.));
#2902=CARTESIAN_POINT('',(48.228498768677,-5.99999999999996,10.));
#2903=CARTESIAN_POINT('',(48.228498768677,6.00000000000004,10.));
#2904=CARTESIAN_POINT('Origin',(48.228498768677,4.16333634234434E-14,-1.99999999999999));
#2905=CARTESIAN_POINT('',(48.228498768677,-11.25,-1.99999999999999));
#2906=CARTESIAN_POINT('',(48.228498768677,11.25,-1.99999999999999));
#2907=CARTESIAN_POINT('Origin',(48.228498768677,4.16333634234434E-14,-1.99999999999999));
#2908=CARTESIAN_POINT('',(48.228498768677,-11.25,-1.99999999999999));
#2909=CARTESIAN_POINT('',(-8.77150123132295,11.2500000000001,-2.));
#2910=CARTESIAN_POINT('',(48.228498768677,-5.99999999999996,-1.99999999999999));
#2911=CARTESIAN_POINT('',(48.228498768677,-5.99999999999996,-1.99999999999999));
#2912=CARTESIAN_POINT('',(48.228498768677,6.00000000000004,-1.99999999999999));
#2913=CARTESIAN_POINT('Origin',(48.228498768677,4.16333634234434E-14,-1.99999999999999));
#2914=CARTESIAN_POINT('',(48.228498768677,6.00000000000004,-1.99999999999999));
#2915=CARTESIAN_POINT('Origin',(48.228498768677,4.16333634234434E-14,10.));
#2916=CARTESIAN_POINT('',(48.228498768677,11.25,10.));
#2917=CARTESIAN_POINT('',(48.228498768677,-11.25,10.));
#2918=CARTESIAN_POINT('Origin',(-8.77150123132294,11.2500000000001,10.));
#2919=CARTESIAN_POINT('Origin',(48.228498768677,-11.25,10.));
#2920=CARTESIAN_POINT('Origin',(48.228498768677,4.16333634234434E-14,10.));
#2921=CARTESIAN_POINT('',(48.228498768677,-5.99999999999996,10.));
#2922=CARTESIAN_POINT('',(48.228498768677,6.00000000000004,10.));
#2923=CARTESIAN_POINT('Origin',(48.228498768677,6.00000000000004,10.));
#2924=CARTESIAN_POINT('Origin',(48.228498768677,-5.99999999999996,10.));
#2925=CARTESIAN_POINT('',(0.,0.,0.));
#2926=CARTESIAN_POINT('Origin',(52.0832482616116,41.2500000000001,10.3911166878577));
#2927=CARTESIAN_POINT('',(56.5832482616116,41.2500000000001,10.3911166878577));
#2928=CARTESIAN_POINT('Origin',(52.0832482616116,41.2500000000001,10.3911166878577));
#2929=CARTESIAN_POINT('',(56.5832482616116,41.2500000000001,-3.10888331214233));
#2930=CARTESIAN_POINT('',(56.5832482616116,41.2500000000001,10.3911166878577));
#2931=CARTESIAN_POINT('Origin',(52.0832482616116,41.2500000000001,-3.10888331214233));
#2932=CARTESIAN_POINT('Origin',(52.0832482616116,3.75000000000002,10.3911166878578));
#2933=CARTESIAN_POINT('',(56.5832482616116,3.75000000000002,10.3911166878578));
#2934=CARTESIAN_POINT('Origin',(52.0832482616116,3.75000000000002,10.3911166878578));
#2935=CARTESIAN_POINT('',(56.5832482616116,3.75000000000002,-3.10888331214225));
#2936=CARTESIAN_POINT('',(56.5832482616116,3.75000000000002,10.3911166878578));
#2937=CARTESIAN_POINT('Origin',(52.0832482616116,3.75,-3.10888331214225));
#2938=CARTESIAN_POINT('Origin',(52.0832482616116,22.5,10.3911166878578));
#2939=CARTESIAN_POINT('',(56.5832482616116,22.5,10.3911166878578));
#2940=CARTESIAN_POINT('Origin',(52.0832482616116,22.5,10.3911166878578));
#2941=CARTESIAN_POINT('',(56.5832482616116,22.5,-3.10888331214233));
#2942=CARTESIAN_POINT('',(56.5832482616116,22.5,10.3911166878578));
#2943=CARTESIAN_POINT('Origin',(52.0832482616116,22.5,-3.10888331214233));
#2944=CARTESIAN_POINT('Origin',(8.5832482616116,22.5,10.3911166878578));
#2945=CARTESIAN_POINT('',(13.0832482616116,22.5,10.3911166878578));
#2946=CARTESIAN_POINT('Origin',(8.5832482616116,22.5,10.3911166878578));
#2947=CARTESIAN_POINT('',(13.0832482616116,22.5,-3.10888331214233));
#2948=CARTESIAN_POINT('',(13.0832482616116,22.5,10.3911166878578));
#2949=CARTESIAN_POINT('Origin',(8.5832482616116,22.5,-3.10888331214233));
#2950=CARTESIAN_POINT('Origin',(8.58324826161155,3.75000000000002,10.3911166878578));
#2951=CARTESIAN_POINT('',(12.3332482616116,3.75000000000002,10.3911166878578));
#2952=CARTESIAN_POINT('Origin',(8.58324826161155,3.75000000000002,10.3911166878578));
#2953=CARTESIAN_POINT('',(12.3332482616116,3.75000000000002,-3.10888331214225));
#2954=CARTESIAN_POINT('',(12.3332482616116,3.75000000000002,10.3911166878578));
#2955=CARTESIAN_POINT('Origin',(8.5832482616116,3.75,-3.10888331214225));
#2956=CARTESIAN_POINT('Origin',(8.5832482616116,41.2500000000001,10.3911166878578));
#2957=CARTESIAN_POINT('',(12.3332482616116,41.2500000000001,10.3911166878578));
#2958=CARTESIAN_POINT('Origin',(8.5832482616116,41.2500000000001,10.3911166878578));
#2959=CARTESIAN_POINT('',(12.3332482616116,41.2500000000001,-3.10888331214233));
#2960=CARTESIAN_POINT('',(12.3332482616116,41.2500000000001,10.3911166878578));
#2961=CARTESIAN_POINT('Origin',(8.5832482616116,41.2500000000001,-3.10888331214233));
#2962=CARTESIAN_POINT('Origin',(-13.9167517383884,-11.25,10.3911166878578));
#2963=CARTESIAN_POINT('',(-6.41675173838841,56.25,10.3911166878578));
#2964=CARTESIAN_POINT('',(-6.41675173838841,-11.25,10.3911166878578));
#2965=CARTESIAN_POINT('',(-6.41675173838841,-11.25,10.3911166878578));
#2966=CARTESIAN_POINT('',(23.5832482616121,-11.25,10.3911166878578));
#2967=CARTESIAN_POINT('',(-13.9167517383884,-11.25,10.3911166878578));
#2968=CARTESIAN_POINT('',(23.5832482616121,56.25,10.3911166878578));
#2969=CARTESIAN_POINT('',(23.5832482616121,-11.25,10.3911166878578));
#2970=CARTESIAN_POINT('',(68.5832482616116,56.25,10.3911166878577));
#2971=CARTESIAN_POINT('Origin',(-13.9167517383884,-11.25,10.3911166878578));
#2972=CARTESIAN_POINT('',(61.0832482616116,-11.25,10.3911166878578));
#2973=CARTESIAN_POINT('',(61.0832482616116,56.25,10.3911166878577));
#2974=CARTESIAN_POINT('',(61.0832482616116,-11.25,10.3911166878578));
#2975=CARTESIAN_POINT('',(43.0832482616116,56.25,10.3911166878577));
#2976=CARTESIAN_POINT('',(68.5832482616116,56.25,10.3911166878577));
#2977=CARTESIAN_POINT('',(43.0832482616116,-11.25,10.3911166878578));
#2978=CARTESIAN_POINT('',(43.0832482616116,-11.25,10.3911166878578));
#2979=CARTESIAN_POINT('',(-13.9167517383884,-11.25,10.3911166878578));
#2980=CARTESIAN_POINT('Origin',(-13.9167517383884,-11.25,-3.10888331214225));
#2981=CARTESIAN_POINT('',(68.5832482616116,-11.25,-3.10888331214226));
#2982=CARTESIAN_POINT('',(68.5832482616116,56.2500000000001,-3.10888331214233));
#2983=CARTESIAN_POINT('',(68.5832482616116,-11.25,-3.10888331214226));
#2984=CARTESIAN_POINT('',(-13.9167517383884,-11.25,-3.10888331214225));
#2985=CARTESIAN_POINT('',(-13.9167517383884,-11.25,-3.10888331214225));
#2986=CARTESIAN_POINT('',(-13.9167517383884,56.2500000000001,-3.10888331214232));
#2987=CARTESIAN_POINT('',(-13.9167517383884,56.2500000000001,-3.10888331214232));
#2988=CARTESIAN_POINT('',(68.5832482616116,56.2500000000001,-3.10888331214233));
#2989=CARTESIAN_POINT('Origin',(68.5832482616116,-11.25,10.3911166878578));
#2990=CARTESIAN_POINT('',(68.5832482616116,56.2500000000001,19.3911166878577));
#2991=CARTESIAN_POINT('',(68.5832482616116,56.25,10.3911166878577));
#2992=CARTESIAN_POINT('',(68.5832482616116,-11.25,19.3911166878577));
#2993=CARTESIAN_POINT('',(68.5832482616116,-11.25,19.3911166878577));
#2994=CARTESIAN_POINT('',(68.5832482616116,-11.25,10.3911166878578));
#2995=CARTESIAN_POINT('Origin',(68.5832482616116,56.25,10.3911166878577));
#2996=CARTESIAN_POINT('',(-13.9167517383884,56.2500000000001,19.3911166878577));
#2997=CARTESIAN_POINT('',(-13.9167517383884,56.25,10.3911166878578));
#2998=CARTESIAN_POINT('',(-6.41675173838841,56.2500000000001,19.3911166878577));
#2999=CARTESIAN_POINT('',(-13.9167517383884,56.2500000000001,19.3911166878577));
#3000=CARTESIAN_POINT('',(-6.41675173838841,56.2500000000001,19.3911166878577));
#3001=CARTESIAN_POINT('',(23.5832482616121,56.2500000000001,19.3911166878577));
#3002=CARTESIAN_POINT('',(23.5832482616121,56.2500000000001,19.3911166878577));
#3003=CARTESIAN_POINT('',(43.0832482616116,56.2500000000001,19.3911166878577));
#3004=CARTESIAN_POINT('',(-13.9167517383884,56.2500000000001,19.3911166878577));
#3005=CARTESIAN_POINT('',(43.0832482616116,56.2500000000001,19.3911166878577));
#3006=CARTESIAN_POINT('',(61.0832482616116,56.2500000000001,19.3911166878577));
#3007=CARTESIAN_POINT('',(61.0832482616116,56.2500000000001,19.3911166878577));
#3008=CARTESIAN_POINT('',(-13.9167517383884,56.2500000000001,19.3911166878577));
#3009=CARTESIAN_POINT('Origin',(-13.9167517383884,56.25,10.3911166878578));
#3010=CARTESIAN_POINT('',(-13.9167517383884,-11.25,19.3911166878577));
#3011=CARTESIAN_POINT('',(-13.9167517383884,-11.25,10.3911166878578));
#3012=CARTESIAN_POINT('',(-13.9167517383884,-11.25,19.3911166878577));
#3013=CARTESIAN_POINT('Origin',(-13.9167517383884,-11.25,10.3911166878578));
#3014=CARTESIAN_POINT('',(61.0832482616116,-11.25,19.3911166878577));
#3015=CARTESIAN_POINT('',(-13.9167517383884,-11.25,19.3911166878577));
#3016=CARTESIAN_POINT('',(61.0832482616116,-11.25,19.3911166878577));
#3017=CARTESIAN_POINT('',(43.0832482616116,-11.25,19.3911166878577));
#3018=CARTESIAN_POINT('',(43.0832482616116,-11.25,19.3911166878577));
#3019=CARTESIAN_POINT('',(23.5832482616121,-11.25,19.3911166878578));
#3020=CARTESIAN_POINT('',(-13.9167517383884,-11.25,19.3911166878577));
#3021=CARTESIAN_POINT('',(23.5832482616121,-11.25,19.3911166878578));
#3022=CARTESIAN_POINT('',(-6.41675173838841,-11.25,19.3911166878578));
#3023=CARTESIAN_POINT('',(-6.41675173838841,-11.25,19.3911166878578));
#3024=CARTESIAN_POINT('',(-13.9167517383884,-11.25,19.3911166878577));
#3025=CARTESIAN_POINT('Origin',(23.5832482616121,-11.25,19.3911166878578));
#3026=CARTESIAN_POINT('',(23.5832482616121,-11.25,19.3911166878578));
#3027=CARTESIAN_POINT('Origin',(43.0832482616116,-11.25,19.3911166878577));
#3028=CARTESIAN_POINT('',(43.0832482616116,-11.25,19.3911166878577));
#3029=CARTESIAN_POINT('Origin',(-13.9167517383884,-11.25,19.3911166878577));
#3030=CARTESIAN_POINT('Origin',(-6.41675173838841,-11.25,19.3911166878578));
#3031=CARTESIAN_POINT('',(-6.41675173838841,-11.25,19.3911166878578));
#3032=CARTESIAN_POINT('Origin',(-13.9167517383884,-11.25,19.3911166878577));
#3033=CARTESIAN_POINT('Origin',(61.0832482616116,-11.25,19.3911166878577));
#3034=CARTESIAN_POINT('',(61.0832482616116,-11.25,19.3911166878577));
#3035=CARTESIAN_POINT('Origin',(-13.9167517383884,-11.25,19.3911166878577));
#3036=CARTESIAN_POINT('',(0.,0.,0.));
#3037=CARTESIAN_POINT('Origin',(22.5,25.,27.4190038418755));
#3038=CARTESIAN_POINT('',(22.5,3.99999999999999,31.9190038418755));
#3039=CARTESIAN_POINT('Origin',(22.5,3.99999999999999,27.4190038418755));
#3040=CARTESIAN_POINT('',(22.5,-5.,31.9190038418755));
#3041=CARTESIAN_POINT('',(22.5,25.,31.9190038418755));
#3042=CARTESIAN_POINT('Origin',(22.5,-5.,27.4190038418755));
#3043=CARTESIAN_POINT('Origin',(22.5,25.,27.4190038418755));
#3044=CARTESIAN_POINT('',(22.5,25.,31.9190038418755));
#3045=CARTESIAN_POINT('Origin',(22.5,25.,27.4190038418755));
#3046=CARTESIAN_POINT('',(22.5,16.,31.9190038418755));
#3047=CARTESIAN_POINT('',(22.5,25.,31.9190038418755));
#3048=CARTESIAN_POINT('Origin',(22.5,16.,27.4190038418755));
#3049=CARTESIAN_POINT('Origin',(41.25,10.,7.91900384187549));
#3050=CARTESIAN_POINT('',(45.75,10.,7.91900384187549));
#3051=CARTESIAN_POINT('Origin',(41.25,10.,7.91900384187549));
#3052=CARTESIAN_POINT('',(45.75,10.,-4.0809961581245));
#3053=CARTESIAN_POINT('',(45.75,10.,7.91900384187549));
#3054=CARTESIAN_POINT('Origin',(41.25,10.,-4.0809961581245));
#3055=CARTESIAN_POINT('Origin',(3.74999999999999,10.,7.91900384187547));
#3056=CARTESIAN_POINT('',(8.25,10.,7.91900384187547));
#3057=CARTESIAN_POINT('Origin',(3.74999999999999,10.,7.91900384187547));
#3058=CARTESIAN_POINT('',(8.25,10.,-4.08099615812454));
#3059=CARTESIAN_POINT('',(8.25,10.,7.91900384187547));
#3060=CARTESIAN_POINT('Origin',(3.74999999999999,10.,-4.08099615812454));
#3061=CARTESIAN_POINT('Origin',(-11.25,-5.,36.4190038418755));
#3062=CARTESIAN_POINT('',(14.25,-5.,36.4190038418755));
#3063=CARTESIAN_POINT('',(30.7500000000001,-5.,36.4190038418755));
#3064=CARTESIAN_POINT('',(33.75,-5.,36.4190038418755));
#3065=CARTESIAN_POINT('',(30.7500000000001,3.99999999999999,36.4190038418755));
#3066=CARTESIAN_POINT('',(30.7500000000001,-5.,36.4190038418755));
#3067=CARTESIAN_POINT('',(14.25,3.99999999999999,36.4190038418755));
#3068=CARTESIAN_POINT('',(-11.25,3.99999999999999,36.4190038418755));
#3069=CARTESIAN_POINT('',(14.25,-5.,36.4190038418755));
#3070=CARTESIAN_POINT('Origin',(-11.2500000000001,-5.,7.91900384187547));
#3071=CARTESIAN_POINT('',(33.75,-5.,7.91900384187549));
#3072=CARTESIAN_POINT('',(33.75,25.,7.91900384187549));
#3073=CARTESIAN_POINT('',(33.75,25.,7.91900384187549));
#3074=CARTESIAN_POINT('',(56.2500000000001,-5.,7.91900384187549));
#3075=CARTESIAN_POINT('',(-11.2500000000001,-5.,7.91900384187547));
#3076=CARTESIAN_POINT('',(56.2500000000001,25.,7.91900384187549));
#3077=CARTESIAN_POINT('',(56.2500000000001,-5.,7.91900384187549));
#3078=CARTESIAN_POINT('',(56.2500000000001,25.,7.91900384187549));
#3079=CARTESIAN_POINT('Origin',(-11.2500000000001,-5.,7.91900384187547));
#3080=CARTESIAN_POINT('',(11.25,25.,7.91900384187549));
#3081=CARTESIAN_POINT('',(11.25,-5.,7.91900384187549));
#3082=CARTESIAN_POINT('',(11.25,25.,7.91900384187549));
#3083=CARTESIAN_POINT('',(-11.2500000000001,25.,7.91900384187547));
#3084=CARTESIAN_POINT('',(56.2500000000001,25.,7.91900384187549));
#3085=CARTESIAN_POINT('',(-11.2500000000001,-5.,7.91900384187547));
#3086=CARTESIAN_POINT('',(-11.2500000000001,25.,7.91900384187547));
#3087=CARTESIAN_POINT('',(-11.2500000000001,-5.,7.91900384187547));
#3088=CARTESIAN_POINT('Origin',(-11.25,-5.,-4.08099615812456));
#3089=CARTESIAN_POINT('',(-11.25,25.,-4.08099615812456));
#3090=CARTESIAN_POINT('',(-11.25,-5.,-4.08099615812456));
#3091=CARTESIAN_POINT('',(-11.25,25.,-4.08099615812456));
#3092=CARTESIAN_POINT('',(56.2500000000001,25.,-4.08099615812452));
#3093=CARTESIAN_POINT('',(3.74999999999999,25.,-4.08099615812456));
#3094=CARTESIAN_POINT('',(56.2500000000001,-5.,-4.0809961581245));
#3095=CARTESIAN_POINT('',(56.2500000000001,-5.,-4.0809961581245));
#3096=CARTESIAN_POINT('',(-11.25,-5.,-4.08099615812456));
#3097=CARTESIAN_POINT('Origin',(-11.2500000000001,25.,7.91900384187547));
#3098=CARTESIAN_POINT('',(-11.2500000000001,-5.,7.91900384187547));
#3099=CARTESIAN_POINT('',(-11.2500000000001,25.,7.91900384187547));
#3100=CARTESIAN_POINT('Origin',(-11.2500000000001,-5.,7.91900384187547));
#3101=CARTESIAN_POINT('',(33.75,-5.,33.4190038418755));
#3102=CARTESIAN_POINT('',(33.75,-5.,36.4190038418755));
#3103=CARTESIAN_POINT('Origin',(30.75,-5.,33.4190038418756));
#3104=CARTESIAN_POINT('',(11.25,-5.,33.4190038418756));
#3105=CARTESIAN_POINT('Origin',(14.25,-5.,33.4190038418756));
#3106=CARTESIAN_POINT('',(11.25,-5.,36.4190038418755));
#3107=CARTESIAN_POINT('',(56.2500000000001,-5.,7.91900384187549));
#3108=CARTESIAN_POINT('Origin',(56.2500000000001,-5.,7.91900384187549));
#3109=CARTESIAN_POINT('',(56.2500000000001,25.,7.91900384187549));
#3110=CARTESIAN_POINT('Origin',(3.74999999999999,25.,7.91900384187547));
#3111=CARTESIAN_POINT('',(30.7500000000001,25.,36.4190038418755));
#3112=CARTESIAN_POINT('',(14.25,25.,36.4190038418755));
#3113=CARTESIAN_POINT('',(11.25,25.,36.4190038418756));
#3114=CARTESIAN_POINT('',(33.75,25.,33.4190038418756));
#3115=CARTESIAN_POINT('Origin',(30.75,25.,33.4190038418756));
#3116=CARTESIAN_POINT('',(33.75,25.,36.4190038418755));
#3117=CARTESIAN_POINT('',(11.25,25.,33.4190038418756));
#3118=CARTESIAN_POINT('',(11.25,25.,36.4190038418756));
#3119=CARTESIAN_POINT('Origin',(14.25,25.,33.4190038418756));
#3120=CARTESIAN_POINT('Origin',(11.25,25.,36.4190038418756));
#3121=CARTESIAN_POINT('',(11.25,16.,13.9190038418755));
#3122=CARTESIAN_POINT('',(11.25,16.,33.4190038418756));
#3123=CARTESIAN_POINT('',(11.25,16.,13.9190038418755));
#3124=CARTESIAN_POINT('',(11.25,25.,33.4190038418756));
#3125=CARTESIAN_POINT('',(11.25,3.99999999999999,33.4190038418756));
#3126=CARTESIAN_POINT('',(11.25,25.,33.4190038418756));
#3127=CARTESIAN_POINT('',(11.25,4.,13.9190038418755));
#3128=CARTESIAN_POINT('',(11.25,4.,13.9190038418755));
#3129=CARTESIAN_POINT('',(11.25,-5.,13.9190038418755));
#3130=CARTESIAN_POINT('Origin',(33.75,25.,36.4190038418755));
#3131=CARTESIAN_POINT('',(33.75,16.,33.4190038418755));
#3132=CARTESIAN_POINT('',(33.75,25.,33.4190038418756));
#3133=CARTESIAN_POINT('',(33.75,16.,13.9190038418755));
#3134=CARTESIAN_POINT('',(33.75,16.,13.9190038418755));
#3135=CARTESIAN_POINT('',(33.75,4.,13.9190038418755));
#3136=CARTESIAN_POINT('',(33.7500000000001,-5.,13.9190038418755));
#3137=CARTESIAN_POINT('',(33.75,3.99999999999999,33.4190038418755));
#3138=CARTESIAN_POINT('',(33.75,4.,13.9190038418755));
#3139=CARTESIAN_POINT('',(33.75,25.,33.4190038418756));
#3140=CARTESIAN_POINT('Origin',(-11.25,-5.,36.4190038418755));
#3141=CARTESIAN_POINT('',(30.7500000000001,16.,36.4190038418755));
#3142=CARTESIAN_POINT('',(14.25,16.,36.4190038418755));
#3143=CARTESIAN_POINT('',(-11.25,16.,36.4190038418755));
#3144=CARTESIAN_POINT('',(30.7500000000001,-5.,36.4190038418755));
#3145=CARTESIAN_POINT('',(14.25,-5.,36.4190038418755));
#3146=CARTESIAN_POINT('Origin',(-11.2500000000001,4.,13.9190038418755));
#3147=CARTESIAN_POINT('Origin',(30.75,3.99999999999999,33.4190038418756));
#3148=CARTESIAN_POINT('',(-11.2500000000001,4.,13.9190038418755));
#3149=CARTESIAN_POINT('Origin',(14.25,3.99999999999999,33.4190038418756));
#3150=CARTESIAN_POINT('Origin',(-11.2500000000001,16.,13.9190038418755));
#3151=CARTESIAN_POINT('Origin',(30.75,16.,33.4190038418756));
#3152=CARTESIAN_POINT('Origin',(14.25,16.,33.4190038418756));
#3153=CARTESIAN_POINT('',(-11.2500000000001,16.,13.9190038418755));
#3154=CARTESIAN_POINT('Origin',(-11.2500000000001,-5.,13.9190038418755));
#3155=CARTESIAN_POINT('Origin',(30.75,-5.,33.4190038418756));
#3156=CARTESIAN_POINT('Origin',(30.75,-5.,33.4190038418756));
#3157=CARTESIAN_POINT('Origin',(14.25,-5.,33.4190038418756));
#3158=CARTESIAN_POINT('Origin',(14.25,-5.,33.4190038418756));
#3159=CARTESIAN_POINT('',(0.,0.,0.));
#3160=CARTESIAN_POINT('Origin',(-3.46944695195361E-15,29.04,1.38777878078145E-14));
#3161=CARTESIAN_POINT('',(-3.77073783102926E-15,29.04,4.50000000000003));
#3162=CARTESIAN_POINT('Origin',(-3.46944695195361E-15,29.04,1.38777878078145E-14));
#3163=CARTESIAN_POINT('',(-3.70646244349312E-15,30.,3.54000000000001));
#3164=CARTESIAN_POINT('',(-3.77073783102926E-15,29.04,4.50000000000003));
#3165=CARTESIAN_POINT('Origin',(-3.46944695195361E-15,30.,1.38777878078145E-14));
#3166=CARTESIAN_POINT('Origin',(0.,-5.99999999999999,0.));
#3167=CARTESIAN_POINT('',(8.00891240156965E-16,-5.03999999999999,4.5));
#3168=CARTESIAN_POINT('',(-8.00891240156971E-16,-5.03999999999998,-4.50000000000001));
#3169=CARTESIAN_POINT('Origin',(0.,-5.03999999999999,0.));
#3170=CARTESIAN_POINT('Origin',(0.,-5.03999999999999,0.));
#3171=CARTESIAN_POINT('',(-6.30034442256817E-16,-5.99999999999999,-3.54000000000001));
#3172=CARTESIAN_POINT('',(-6.30034442256817E-16,-5.99999999999999,-3.54000000000001));
#3173=CARTESIAN_POINT('Origin',(0.,-5.99999999999999,0.));
#3174=CARTESIAN_POINT('Origin',(0.,-5.99999999999999,0.));
#3175=CARTESIAN_POINT('',(-3.01290879075651E-16,-5.99999999999999,4.50000000000002));
#3176=CARTESIAN_POINT('Origin',(4.50000000000004,-5.99999999999999,2.08166817117217E-14));
#3177=CARTESIAN_POINT('Origin',(-3.46944695195361E-15,30.,1.38777878078145E-14));
#3178=CARTESIAN_POINT('',(23.8136057910413,1.38464269512253,48.));
#3179=CARTESIAN_POINT('',(-34.6180743514041,37.3895452946904,46.9340563277267));
#3180=CARTESIAN_POINT('',(31.2219059673625,1.43794319442046,48.0464461260994));
#3181=CARTESIAN_POINT('',(1.88192564859591,54.6390127572857,68.9329530282276));
#3182=CARTESIAN_POINT('',(-15.6180743514041,1.54749094412769,48.0148319973984));
#3183=CARTESIAN_POINT('',(-51.6180743514041,28.6186146716517,46.8340070551584));
#3184=CARTESIAN_POINT('',(-56.2013226130157,78.5960796609871,23.2035446839605));
#3185=CARTESIAN_POINT('',(-57.6180743514041,65.4627418297619,68.6123267380715));
#3186=CARTESIAN_POINT('',(-19.1180743514041,-20.973202139575,45.665196409535));
#3187=UNCERTAINTY_MEASURE_WITH_UNIT(LENGTH_MEASURE(0.01),#3207,
'DISTANCE_ACCURACY_VALUE',
'Maximum model space distance between geometric entities at asserted c
onnectivities');
#3188=UNCERTAINTY_MEASURE_WITH_UNIT(LENGTH_MEASURE(0.01),#3207,
'DISTANCE_ACCURACY_VALUE',
'Maximum model space distance between geometric entities at asserted c
onnectivities');
#3189=UNCERTAINTY_MEASURE_WITH_UNIT(LENGTH_MEASURE(0.01),#3207,
'DISTANCE_ACCURACY_VALUE',
'Maximum model space distance between geometric entities at asserted c
onnectivities');
#3190=UNCERTAINTY_MEASURE_WITH_UNIT(LENGTH_MEASURE(0.01),#3207,
'DISTANCE_ACCURACY_VALUE',
'Maximum model space distance between geometric entities at asserted c
onnectivities');
#3191=UNCERTAINTY_MEASURE_WITH_UNIT(LENGTH_MEASURE(0.01),#3207,
'DISTANCE_ACCURACY_VALUE',
'Maximum model space distance between geometric entities at asserted c
onnectivities');
#3192=UNCERTAINTY_MEASURE_WITH_UNIT(LENGTH_MEASURE(0.01),#3207,
'DISTANCE_ACCURACY_VALUE',
'Maximum model space distance between geometric entities at asserted c
onnectivities');
#3193=UNCERTAINTY_MEASURE_WITH_UNIT(LENGTH_MEASURE(0.01),#3207,
'DISTANCE_ACCURACY_VALUE',
'Maximum model space distance between geometric entities at asserted c
onnectivities');
#3194=UNCERTAINTY_MEASURE_WITH_UNIT(LENGTH_MEASURE(0.01),#3207,
'DISTANCE_ACCURACY_VALUE',
'Maximum model space distance between geometric entities at asserted c
onnectivities');
#3195=UNCERTAINTY_MEASURE_WITH_UNIT(LENGTH_MEASURE(0.01),#3207,
'DISTANCE_ACCURACY_VALUE',
'Maximum model space distance between geometric entities at asserted c
onnectivities');
#3196=UNCERTAINTY_MEASURE_WITH_UNIT(LENGTH_MEASURE(0.01),#3207,
'DISTANCE_ACCURACY_VALUE',
'Maximum model space distance between geometric entities at asserted c
onnectivities');
#3197=(
GEOMETRIC_REPRESENTATION_CONTEXT(3)
GLOBAL_UNCERTAINTY_ASSIGNED_CONTEXT((#3187))
GLOBAL_UNIT_ASSIGNED_CONTEXT((#3207,#3209,#3210))
REPRESENTATION_CONTEXT('','3D')
);
#3198=(
GEOMETRIC_REPRESENTATION_CONTEXT(3)
GLOBAL_UNCERTAINTY_ASSIGNED_CONTEXT((#3188))
GLOBAL_UNIT_ASSIGNED_CONTEXT((#3207,#3209,#3210))
REPRESENTATION_CONTEXT('','3D')
);
#3199=(
GEOMETRIC_REPRESENTATION_CONTEXT(3)
GLOBAL_UNCERTAINTY_ASSIGNED_CONTEXT((#3189))
GLOBAL_UNIT_ASSIGNED_CONTEXT((#3207,#3209,#3210))
REPRESENTATION_CONTEXT('','3D')
);
#3200=(
GEOMETRIC_REPRESENTATION_CONTEXT(3)
GLOBAL_UNCERTAINTY_ASSIGNED_CONTEXT((#3190))
GLOBAL_UNIT_ASSIGNED_CONTEXT((#3207,#3209,#3210))
REPRESENTATION_CONTEXT('','3D')
);
#3201=(
GEOMETRIC_REPRESENTATION_CONTEXT(3)
GLOBAL_UNCERTAINTY_ASSIGNED_CONTEXT((#3191))
GLOBAL_UNIT_ASSIGNED_CONTEXT((#3207,#3209,#3210))
REPRESENTATION_CONTEXT('','3D')
);
#3202=(
GEOMETRIC_REPRESENTATION_CONTEXT(3)
GLOBAL_UNCERTAINTY_ASSIGNED_CONTEXT((#3192))
GLOBAL_UNIT_ASSIGNED_CONTEXT((#3207,#3209,#3210))
REPRESENTATION_CONTEXT('','3D')
);
#3203=(
GEOMETRIC_REPRESENTATION_CONTEXT(3)
GLOBAL_UNCERTAINTY_ASSIGNED_CONTEXT((#3193))
GLOBAL_UNIT_ASSIGNED_CONTEXT((#3207,#3209,#3210))
REPRESENTATION_CONTEXT('','3D')
);
#3204=(
GEOMETRIC_REPRESENTATION_CONTEXT(3)
GLOBAL_UNCERTAINTY_ASSIGNED_CONTEXT((#3194))
GLOBAL_UNIT_ASSIGNED_CONTEXT((#3207,#3209,#3210))
REPRESENTATION_CONTEXT('','3D')
);
#3205=(
GEOMETRIC_REPRESENTATION_CONTEXT(3)
GLOBAL_UNCERTAINTY_ASSIGNED_CONTEXT((#3195))
GLOBAL_UNIT_ASSIGNED_CONTEXT((#3207,#3209,#3210))
REPRESENTATION_CONTEXT('','3D')
);
#3206=(
GEOMETRIC_REPRESENTATION_CONTEXT(3)
GLOBAL_UNCERTAINTY_ASSIGNED_CONTEXT((#3196))
GLOBAL_UNIT_ASSIGNED_CONTEXT((#3207,#3209,#3210))
REPRESENTATION_CONTEXT('','3D')
);
#3207=(
LENGTH_UNIT()
NAMED_UNIT(*)
SI_UNIT(.MILLI.,.METRE.)
);
#3208=(
LENGTH_UNIT()
NAMED_UNIT(*)
SI_UNIT($,.METRE.)
);
#3209=(
NAMED_UNIT(*)
PLANE_ANGLE_UNIT()
SI_UNIT($,.RADIAN.)
);
#3210=(
NAMED_UNIT(*)
SI_UNIT($,.STERADIAN.)
SOLID_ANGLE_UNIT()
);
#3211=SHAPE_DEFINITION_REPRESENTATION(#3220,#3238);
#3212=SHAPE_DEFINITION_REPRESENTATION(#3221,#3239);
#3213=SHAPE_DEFINITION_REPRESENTATION(#3222,#3240);
#3214=SHAPE_DEFINITION_REPRESENTATION(#3223,#3241);
#3215=SHAPE_DEFINITION_REPRESENTATION(#3224,#3242);
#3216=SHAPE_DEFINITION_REPRESENTATION(#3225,#3243);
#3217=SHAPE_DEFINITION_REPRESENTATION(#3226,#3244);
#3218=SHAPE_DEFINITION_REPRESENTATION(#3227,#3245);
#3219=SHAPE_DEFINITION_REPRESENTATION(#3228,#3246);
#3220=PRODUCT_DEFINITION_SHAPE('',$,#3248);
#3221=PRODUCT_DEFINITION_SHAPE('',$,#3249);
#3222=PRODUCT_DEFINITION_SHAPE('',$,#3250);
#3223=PRODUCT_DEFINITION_SHAPE('',$,#3251);
#3224=PRODUCT_DEFINITION_SHAPE('',$,#3252);
#3225=PRODUCT_DEFINITION_SHAPE('',$,#3253);
#3226=PRODUCT_DEFINITION_SHAPE('',$,#3254);
#3227=PRODUCT_DEFINITION_SHAPE('',$,#3255);
#3228=PRODUCT_DEFINITION_SHAPE('',$,#3256);
#3229=PRODUCT_DEFINITION_SHAPE($,$,#38);
#3230=PRODUCT_DEFINITION_SHAPE($,$,#39);
#3231=PRODUCT_DEFINITION_SHAPE($,$,#40);
#3232=PRODUCT_DEFINITION_SHAPE($,$,#41);
#3233=PRODUCT_DEFINITION_SHAPE($,$,#42);
#3234=PRODUCT_DEFINITION_SHAPE($,$,#43);
#3235=PRODUCT_DEFINITION_SHAPE($,$,#44);
#3236=PRODUCT_DEFINITION_SHAPE($,$,#45);
#3237=PRODUCT_DEFINITION_SHAPE($,$,#46);
#3238=SHAPE_REPRESENTATION('',(#1876,#2066,#2067,#2068,#2069,#2070,#2071,
#2072,#2073,#2074),#3197);
#3239=SHAPE_REPRESENTATION('',(#1877),#3198);
#3240=SHAPE_REPRESENTATION('',(#1903),#3199);
#3241=SHAPE_REPRESENTATION('',(#1925),#3200);
#3242=SHAPE_REPRESENTATION('',(#1949),#3201);
#3243=SHAPE_REPRESENTATION('',(#1961),#3202);
#3244=SHAPE_REPRESENTATION('',(#1983),#3203);
#3245=SHAPE_REPRESENTATION('',(#2016),#3204);
#3246=SHAPE_REPRESENTATION('',(#2055),#3205);
#3247=PRODUCT_DEFINITION_CONTEXT('part definition',#3276,'design');
#3248=PRODUCT_DEFINITION('MAT-015','MAT-015',#3257,#3247);
#3249=PRODUCT_DEFINITION('Shaft','Shaft',#3258,#3247);
#3250=PRODUCT_DEFINITION('roller','Roller',#3259,#3247);
#3251=PRODUCT_DEFINITION('Side plate','Side Plate',#3260,#3247);
#3252=PRODUCT_DEFINITION('Cam Disc','Cam Disc',#3261,#3247);
#3253=PRODUCT_DEFINITION('Slotted lever','Slotted Lever',#3262,#3247);
#3254=PRODUCT_DEFINITION('Base Block','Base Block',#3263,#3247);
#3255=PRODUCT_DEFINITION('Angle Bracket','Angle Bracket',#3264,#3247);
#3256=PRODUCT_DEFINITION('Pin','Pin',#3265,#3247);
#3257=PRODUCT_DEFINITION_FORMATION('',$,#3278);
#3258=PRODUCT_DEFINITION_FORMATION('',$,#3279);
#3259=PRODUCT_DEFINITION_FORMATION('',$,#3280);
#3260=PRODUCT_DEFINITION_FORMATION('',$,#3281);
#3261=PRODUCT_DEFINITION_FORMATION('',$,#3282);
#3262=PRODUCT_DEFINITION_FORMATION('',$,#3283);
#3263=PRODUCT_DEFINITION_FORMATION('',$,#3284);
#3264=PRODUCT_DEFINITION_FORMATION('',$,#3285);
#3265=PRODUCT_DEFINITION_FORMATION('',$,#3286);
#3266=PRODUCT_RELATED_PRODUCT_CATEGORY('MAT-015','MAT-015',(#3278));
#3267=PRODUCT_RELATED_PRODUCT_CATEGORY('Shaft','Shaft',(#3279));
#3268=PRODUCT_RELATED_PRODUCT_CATEGORY('Roller','Roller',(#3280));
#3269=PRODUCT_RELATED_PRODUCT_CATEGORY('Side Plate','Side Plate',(#3281));
#3270=PRODUCT_RELATED_PRODUCT_CATEGORY('Cam Disc','Cam Disc',(#3282));
#3271=PRODUCT_RELATED_PRODUCT_CATEGORY('Slotted Lever','Slotted Lever',
(#3283));
#3272=PRODUCT_RELATED_PRODUCT_CATEGORY('Base Block','Base Block',(#3284));
#3273=PRODUCT_RELATED_PRODUCT_CATEGORY('Angle Bracket','Angle Bracket',
(#3285));
#3274=PRODUCT_RELATED_PRODUCT_CATEGORY('Pin','Pin',(#3286));
#3275=APPLICATION_PROTOCOL_DEFINITION('international standard',
'automotive_design',2009,#3276);
#3276=APPLICATION_CONTEXT(
'Core Data for Automotive Mechanical Design Process');
#3277=PRODUCT_CONTEXT('part definition',#3276,'mechanical');
#3278=PRODUCT('MAT-015','MAT-015','STEP AP214',(#3277));
#3279=PRODUCT('Shaft','Shaft','Shaft',(#3277));
#3280=PRODUCT('roller','Roller',$,(#3277));
#3281=PRODUCT('Side plate','Side Plate','Side plate',(#3277));
#3282=PRODUCT('Cam Disc','Cam Disc',$,(#3277));
#3283=PRODUCT('Slotted lever','Slotted Lever','Slotted lever',(#3277));
#3284=PRODUCT('Base Block','Base Block',$,(#3277));
#3285=PRODUCT('Angle Bracket','Angle Bracket',$,(#3277));
#3286=PRODUCT('Pin','Pin',$,(#3277));
#3287=PRESENTATION_STYLE_ASSIGNMENT((#3291));
#3288=PRESENTATION_STYLE_ASSIGNMENT((#3292));
#3289=PRESENTATION_STYLE_ASSIGNMENT((#3293));
#3290=PRESENTATION_STYLE_ASSIGNMENT((#3294));
#3291=SURFACE_STYLE_USAGE(.BOTH.,#3295);
#3292=SURFACE_STYLE_USAGE(.BOTH.,#3296);
#3293=SURFACE_STYLE_USAGE(.BOTH.,#3297);
#3294=SURFACE_STYLE_USAGE(.BOTH.,#3298);
#3295=SURFACE_SIDE_STYLE('',(#3299));
#3296=SURFACE_SIDE_STYLE('',(#3300));
#3297=SURFACE_SIDE_STYLE('',(#3301));
#3298=SURFACE_SIDE_STYLE('',(#3302));
#3299=SURFACE_STYLE_FILL_AREA(#3303);
#3300=SURFACE_STYLE_FILL_AREA(#3304);
#3301=SURFACE_STYLE_FILL_AREA(#3305);
#3302=SURFACE_STYLE_FILL_AREA(#3306);
#3303=FILL_AREA_STYLE('Steel - Satin',(#3307));
#3304=FILL_AREA_STYLE('Opaque(61,176,222)',(#3308));
#3305=FILL_AREA_STYLE('Opaque(97,158,199)',(#3309));
#3306=FILL_AREA_STYLE('Opaque(227,224,212)',(#3310));
#3307=FILL_AREA_STYLE_COLOUR('Steel - Satin',#3311);
#3308=FILL_AREA_STYLE_COLOUR('Opaque(61,176,222)',#3312);
#3309=FILL_AREA_STYLE_COLOUR('Opaque(97,158,199)',#3313);
#3310=FILL_AREA_STYLE_COLOUR('Opaque(227,224,212)',#3314);
#3311=COLOUR_RGB('Steel - Satin',0.627450980392157,0.627450980392157,0.627450980392157);
#3312=COLOUR_RGB('Opaque(61,176,222)',0.23921568627451,0.690196078431373,
0.870588235294118);
#3313=COLOUR_RGB('Opaque(97,158,199)',0.380392156862745,0.619607843137255,
0.780392156862745);
#3314=COLOUR_RGB('Opaque(227,224,212)',0.890196078431372,0.87843137254902,
0.831372549019608);
ENDSEC;
END-ISO-10303-21;
